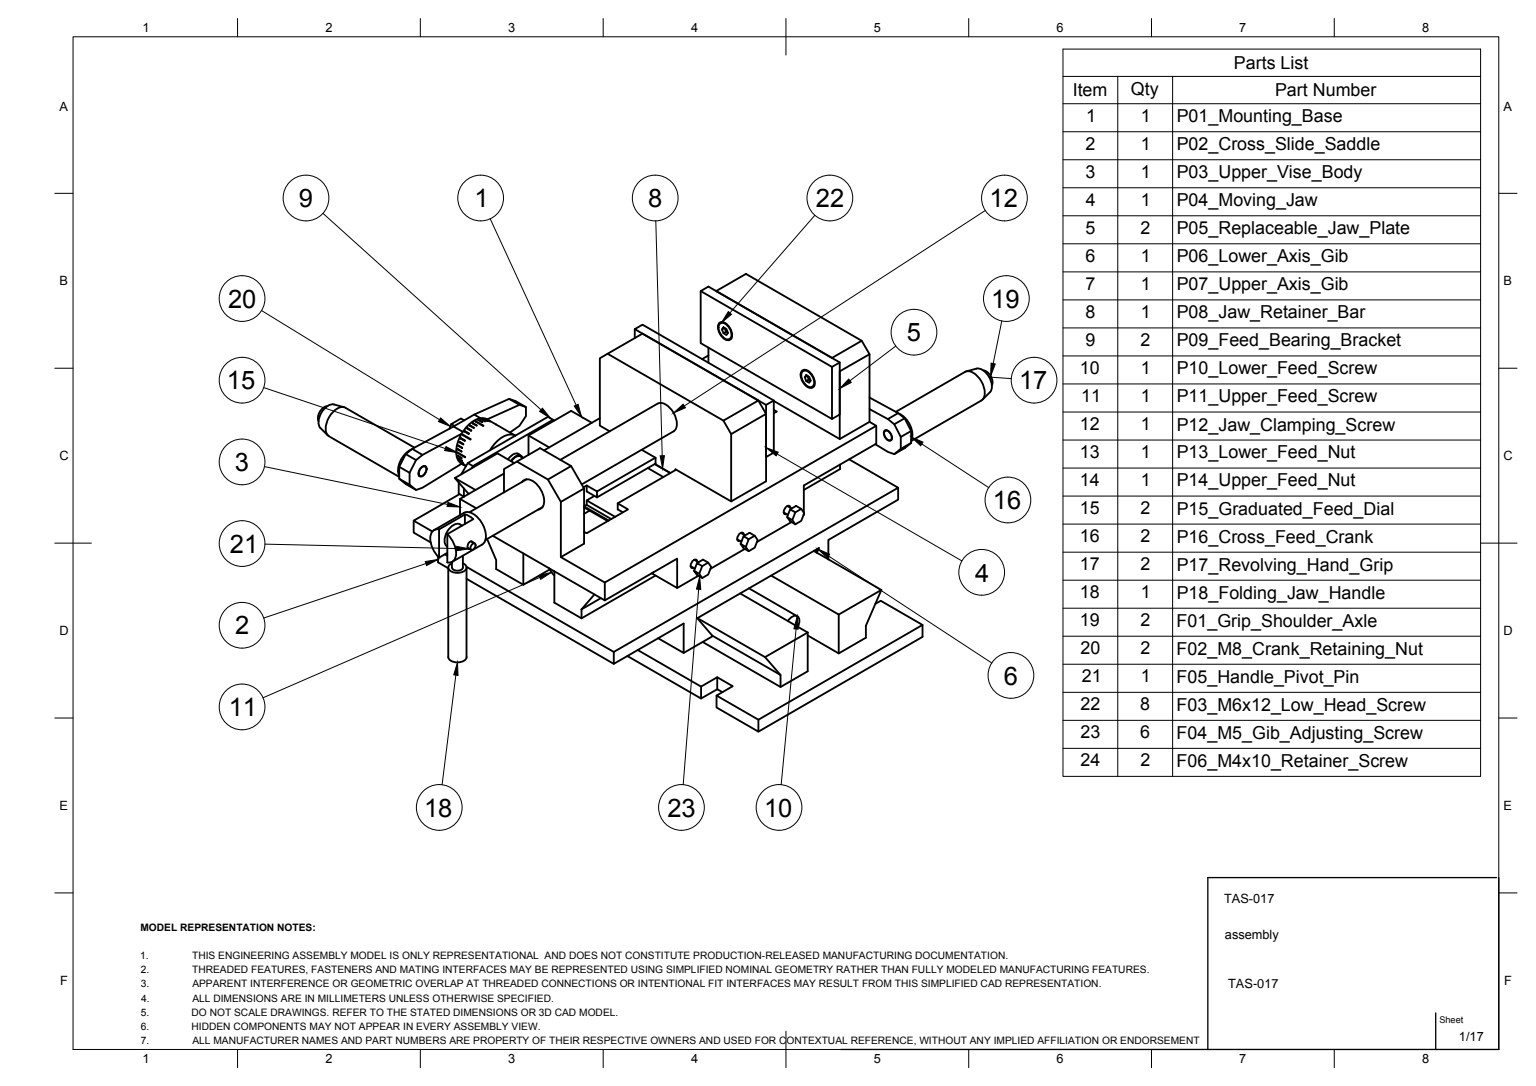
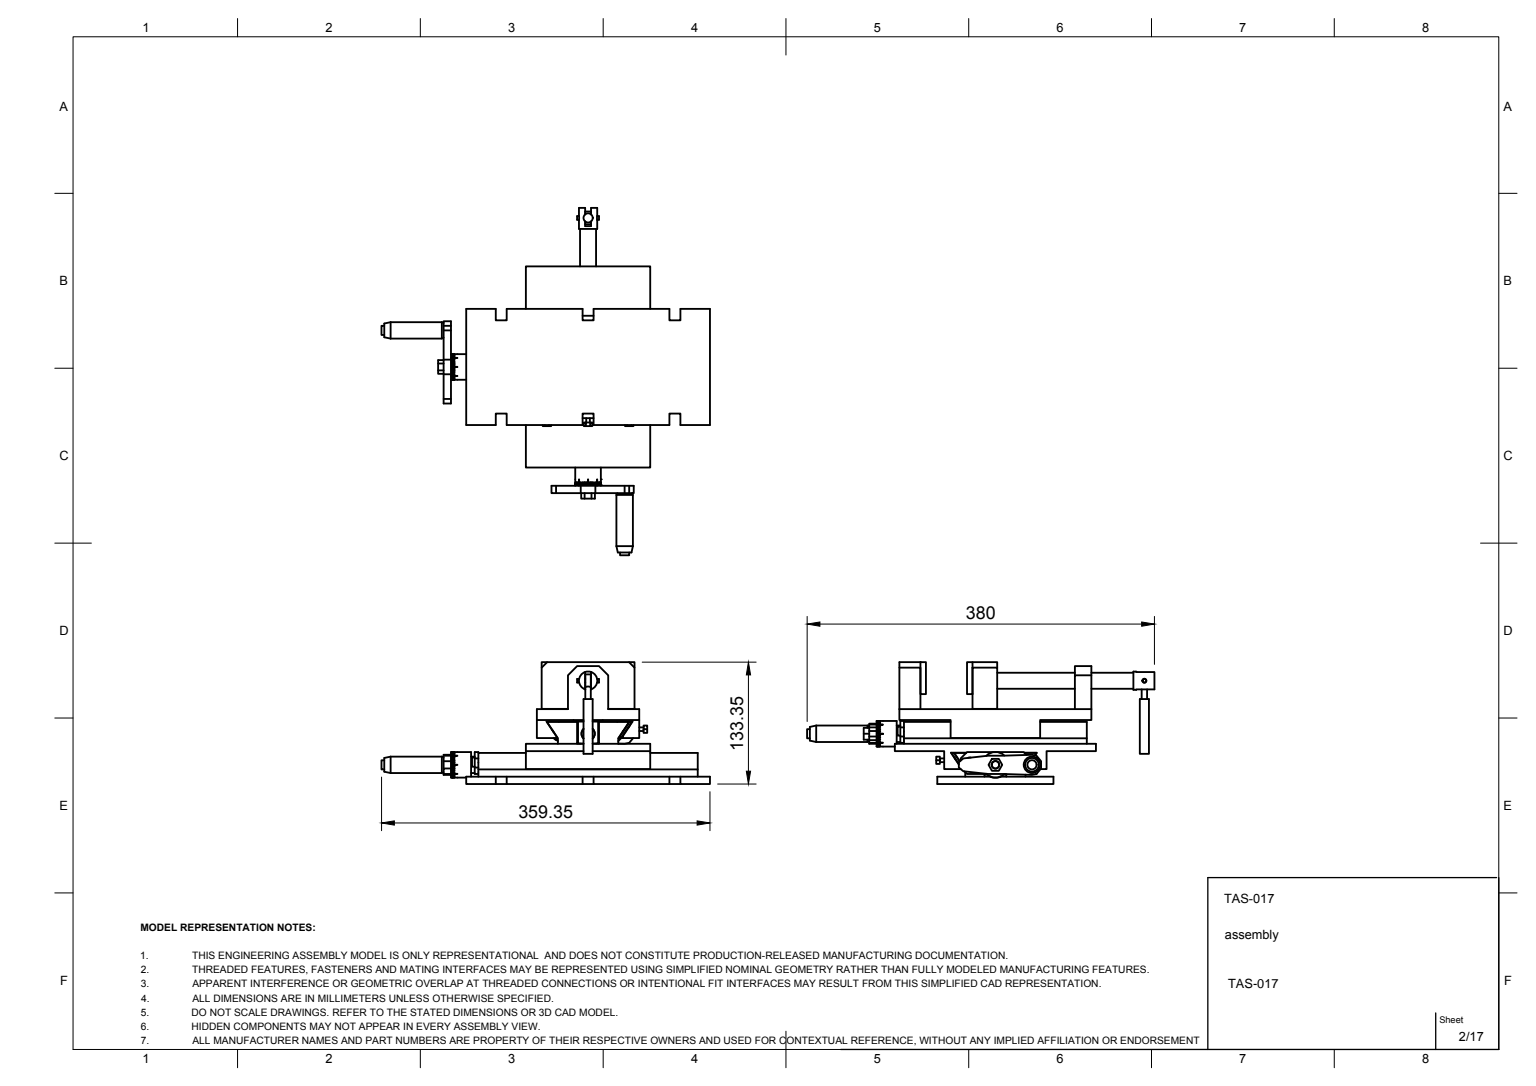
ISO-10303-21;
HEADER;
/* Generated by software containing ST-Developer
 * from STEP Tools, Inc. (www.steptools.com) 
 */

FILE_DESCRIPTION(
/* description */ ('STEP AP203'),
/* implementation_level */ '2;1');

FILE_NAME(
/* name */ 'TAS-017.step',
/* time_stamp */ '2026-11-15T15:04:01-08:00',
/* author */ (''),
/* organization */ (''),
/* preprocessor_version */ 'ST-DEVELOPER v20.2',
/* originating_system */ 'Autodesk Translation Framework v15.17.0.0',
/* authorisation */ '');

FILE_SCHEMA (('AUTOMOTIVE_DESIGN { 1 0 10303 214 3 1 1 }'));
ENDSEC;

DATA;
#10=MECHANICAL_DESIGN_GEOMETRIC_PRESENTATION_REPRESENTATION('',(#276,#277,
#278,#279,#280,#281,#282,#283,#284,#285,#286,#287,#288,#289,#290,#291,#292,
#293,#294,#295,#296,#297,#298,#299,#300,#301,#302,#303,#304,#305),#16598);
#11=ITEM_DEFINED_TRANSFORMATION($,$,#10077,#10884);
#12=ITEM_DEFINED_TRANSFORMATION($,$,#10132,#10885);
#13=ITEM_DEFINED_TRANSFORMATION($,$,#10189,#10886);
#14=ITEM_DEFINED_TRANSFORMATION($,$,#10266,#10887);
#15=ITEM_DEFINED_TRANSFORMATION($,$,#10446,#10888);
#16=ITEM_DEFINED_TRANSFORMATION($,$,#10299,#10889);
#17=ITEM_DEFINED_TRANSFORMATION($,$,#10306,#10890);
#18=ITEM_DEFINED_TRANSFORMATION($,$,#10313,#10891);
#19=ITEM_DEFINED_TRANSFORMATION($,$,#10467,#10892);
#20=ITEM_DEFINED_TRANSFORMATION($,$,#10334,#10893);
#21=ITEM_DEFINED_TRANSFORMATION($,$,#10356,#10894);
#22=ITEM_DEFINED_TRANSFORMATION($,$,#10378,#10895);
#23=ITEM_DEFINED_TRANSFORMATION($,$,#10404,#10896);
#24=ITEM_DEFINED_TRANSFORMATION($,$,#10414,#10897);
#25=ITEM_DEFINED_TRANSFORMATION($,$,#10487,#10898);
#26=ITEM_DEFINED_TRANSFORMATION($,$,#10778,#10899);
#27=ITEM_DEFINED_TRANSFORMATION($,$,#10801,#10900);
#28=ITEM_DEFINED_TRANSFORMATION($,$,#10424,#10901);
#29=ITEM_DEFINED_TRANSFORMATION($,$,#10815,#10902);
#30=ITEM_DEFINED_TRANSFORMATION($,$,#10825,#10903);
#31=ITEM_DEFINED_TRANSFORMATION($,$,#10440,#10904);
#32=ITEM_DEFINED_TRANSFORMATION($,$,#10837,#10905);
#33=ITEM_DEFINED_TRANSFORMATION($,$,#10854,#10906);
#34=ITEM_DEFINED_TRANSFORMATION($,$,#10867,#10907);
#35=ITEM_DEFINED_TRANSFORMATION($,$,#10446,#10908);
#36=ITEM_DEFINED_TRANSFORMATION($,$,#10467,#10909);
#37=ITEM_DEFINED_TRANSFORMATION($,$,#10487,#10910);
#38=ITEM_DEFINED_TRANSFORMATION($,$,#10778,#10911);
#39=ITEM_DEFINED_TRANSFORMATION($,$,#10801,#10912);
#40=ITEM_DEFINED_TRANSFORMATION($,$,#10815,#10913);
#41=ITEM_DEFINED_TRANSFORMATION($,$,#10825,#10914);
#42=ITEM_DEFINED_TRANSFORMATION($,$,#10837,#10915);
#43=ITEM_DEFINED_TRANSFORMATION($,$,#10837,#10916);
#44=ITEM_DEFINED_TRANSFORMATION($,$,#10837,#10917);
#45=ITEM_DEFINED_TRANSFORMATION($,$,#10837,#10918);
#46=ITEM_DEFINED_TRANSFORMATION($,$,#10837,#10919);
#47=ITEM_DEFINED_TRANSFORMATION($,$,#10837,#10920);
#48=ITEM_DEFINED_TRANSFORMATION($,$,#10837,#10921);
#49=ITEM_DEFINED_TRANSFORMATION($,$,#10854,#10922);
#50=ITEM_DEFINED_TRANSFORMATION($,$,#10854,#10923);
#51=ITEM_DEFINED_TRANSFORMATION($,$,#10854,#10924);
#52=ITEM_DEFINED_TRANSFORMATION($,$,#10854,#10925);
#53=ITEM_DEFINED_TRANSFORMATION($,$,#10854,#10926);
#54=ITEM_DEFINED_TRANSFORMATION($,$,#10867,#10927);
#55=(
REPRESENTATION_RELATIONSHIP($,$,#16698,#16697)
REPRESENTATION_RELATIONSHIP_WITH_TRANSFORMATION(#11)
SHAPE_REPRESENTATION_RELATIONSHIP()
);
#56=(
REPRESENTATION_RELATIONSHIP($,$,#16699,#16697)
REPRESENTATION_RELATIONSHIP_WITH_TRANSFORMATION(#12)
SHAPE_REPRESENTATION_RELATIONSHIP()
);
#57=(
REPRESENTATION_RELATIONSHIP($,$,#16700,#16697)
REPRESENTATION_RELATIONSHIP_WITH_TRANSFORMATION(#13)
SHAPE_REPRESENTATION_RELATIONSHIP()
);
#58=(
REPRESENTATION_RELATIONSHIP($,$,#16701,#16697)
REPRESENTATION_RELATIONSHIP_WITH_TRANSFORMATION(#14)
SHAPE_REPRESENTATION_RELATIONSHIP()
);
#59=(
REPRESENTATION_RELATIONSHIP($,$,#16712,#16697)
REPRESENTATION_RELATIONSHIP_WITH_TRANSFORMATION(#15)
SHAPE_REPRESENTATION_RELATIONSHIP()
);
#60=(
REPRESENTATION_RELATIONSHIP($,$,#16702,#16697)
REPRESENTATION_RELATIONSHIP_WITH_TRANSFORMATION(#16)
SHAPE_REPRESENTATION_RELATIONSHIP()
);
#61=(
REPRESENTATION_RELATIONSHIP($,$,#16703,#16697)
REPRESENTATION_RELATIONSHIP_WITH_TRANSFORMATION(#17)
SHAPE_REPRESENTATION_RELATIONSHIP()
);
#62=(
REPRESENTATION_RELATIONSHIP($,$,#16704,#16697)
REPRESENTATION_RELATIONSHIP_WITH_TRANSFORMATION(#18)
SHAPE_REPRESENTATION_RELATIONSHIP()
);
#63=(
REPRESENTATION_RELATIONSHIP($,$,#16713,#16697)
REPRESENTATION_RELATIONSHIP_WITH_TRANSFORMATION(#19)
SHAPE_REPRESENTATION_RELATIONSHIP()
);
#64=(
REPRESENTATION_RELATIONSHIP($,$,#16705,#16697)
REPRESENTATION_RELATIONSHIP_WITH_TRANSFORMATION(#20)
SHAPE_REPRESENTATION_RELATIONSHIP()
);
#65=(
REPRESENTATION_RELATIONSHIP($,$,#16706,#16697)
REPRESENTATION_RELATIONSHIP_WITH_TRANSFORMATION(#21)
SHAPE_REPRESENTATION_RELATIONSHIP()
);
#66=(
REPRESENTATION_RELATIONSHIP($,$,#16707,#16697)
REPRESENTATION_RELATIONSHIP_WITH_TRANSFORMATION(#22)
SHAPE_REPRESENTATION_RELATIONSHIP()
);
#67=(
REPRESENTATION_RELATIONSHIP($,$,#16708,#16697)
REPRESENTATION_RELATIONSHIP_WITH_TRANSFORMATION(#23)
SHAPE_REPRESENTATION_RELATIONSHIP()
);
#68=(
REPRESENTATION_RELATIONSHIP($,$,#16709,#16697)
REPRESENTATION_RELATIONSHIP_WITH_TRANSFORMATION(#24)
SHAPE_REPRESENTATION_RELATIONSHIP()
);
#69=(
REPRESENTATION_RELATIONSHIP($,$,#16714,#16697)
REPRESENTATION_RELATIONSHIP_WITH_TRANSFORMATION(#25)
SHAPE_REPRESENTATION_RELATIONSHIP()
);
#70=(
REPRESENTATION_RELATIONSHIP($,$,#16715,#16697)
REPRESENTATION_RELATIONSHIP_WITH_TRANSFORMATION(#26)
SHAPE_REPRESENTATION_RELATIONSHIP()
);
#71=(
REPRESENTATION_RELATIONSHIP($,$,#16716,#16697)
REPRESENTATION_RELATIONSHIP_WITH_TRANSFORMATION(#27)
SHAPE_REPRESENTATION_RELATIONSHIP()
);
#72=(
REPRESENTATION_RELATIONSHIP($,$,#16710,#16697)
REPRESENTATION_RELATIONSHIP_WITH_TRANSFORMATION(#28)
SHAPE_REPRESENTATION_RELATIONSHIP()
);
#73=(
REPRESENTATION_RELATIONSHIP($,$,#16717,#16697)
REPRESENTATION_RELATIONSHIP_WITH_TRANSFORMATION(#29)
SHAPE_REPRESENTATION_RELATIONSHIP()
);
#74=(
REPRESENTATION_RELATIONSHIP($,$,#16718,#16697)
REPRESENTATION_RELATIONSHIP_WITH_TRANSFORMATION(#30)
SHAPE_REPRESENTATION_RELATIONSHIP()
);
#75=(
REPRESENTATION_RELATIONSHIP($,$,#16711,#16697)
REPRESENTATION_RELATIONSHIP_WITH_TRANSFORMATION(#31)
SHAPE_REPRESENTATION_RELATIONSHIP()
);
#76=(
REPRESENTATION_RELATIONSHIP($,$,#16719,#16697)
REPRESENTATION_RELATIONSHIP_WITH_TRANSFORMATION(#32)
SHAPE_REPRESENTATION_RELATIONSHIP()
);
#77=(
REPRESENTATION_RELATIONSHIP($,$,#16720,#16697)
REPRESENTATION_RELATIONSHIP_WITH_TRANSFORMATION(#33)
SHAPE_REPRESENTATION_RELATIONSHIP()
);
#78=(
REPRESENTATION_RELATIONSHIP($,$,#16721,#16697)
REPRESENTATION_RELATIONSHIP_WITH_TRANSFORMATION(#34)
SHAPE_REPRESENTATION_RELATIONSHIP()
);
#79=(
REPRESENTATION_RELATIONSHIP($,$,#16712,#16697)
REPRESENTATION_RELATIONSHIP_WITH_TRANSFORMATION(#35)
SHAPE_REPRESENTATION_RELATIONSHIP()
);
#80=(
REPRESENTATION_RELATIONSHIP($,$,#16713,#16697)
REPRESENTATION_RELATIONSHIP_WITH_TRANSFORMATION(#36)
SHAPE_REPRESENTATION_RELATIONSHIP()
);
#81=(
REPRESENTATION_RELATIONSHIP($,$,#16714,#16697)
REPRESENTATION_RELATIONSHIP_WITH_TRANSFORMATION(#37)
SHAPE_REPRESENTATION_RELATIONSHIP()
);
#82=(
REPRESENTATION_RELATIONSHIP($,$,#16715,#16697)
REPRESENTATION_RELATIONSHIP_WITH_TRANSFORMATION(#38)
SHAPE_REPRESENTATION_RELATIONSHIP()
);
#83=(
REPRESENTATION_RELATIONSHIP($,$,#16716,#16697)
REPRESENTATION_RELATIONSHIP_WITH_TRANSFORMATION(#39)
SHAPE_REPRESENTATION_RELATIONSHIP()
);
#84=(
REPRESENTATION_RELATIONSHIP($,$,#16717,#16697)
REPRESENTATION_RELATIONSHIP_WITH_TRANSFORMATION(#40)
SHAPE_REPRESENTATION_RELATIONSHIP()
);
#85=(
REPRESENTATION_RELATIONSHIP($,$,#16718,#16697)
REPRESENTATION_RELATIONSHIP_WITH_TRANSFORMATION(#41)
SHAPE_REPRESENTATION_RELATIONSHIP()
);
#86=(
REPRESENTATION_RELATIONSHIP($,$,#16719,#16697)
REPRESENTATION_RELATIONSHIP_WITH_TRANSFORMATION(#42)
SHAPE_REPRESENTATION_RELATIONSHIP()
);
#87=(
REPRESENTATION_RELATIONSHIP($,$,#16719,#16697)
REPRESENTATION_RELATIONSHIP_WITH_TRANSFORMATION(#43)
SHAPE_REPRESENTATION_RELATIONSHIP()
);
#88=(
REPRESENTATION_RELATIONSHIP($,$,#16719,#16697)
REPRESENTATION_RELATIONSHIP_WITH_TRANSFORMATION(#44)
SHAPE_REPRESENTATION_RELATIONSHIP()
);
#89=(
REPRESENTATION_RELATIONSHIP($,$,#16719,#16697)
REPRESENTATION_RELATIONSHIP_WITH_TRANSFORMATION(#45)
SHAPE_REPRESENTATION_RELATIONSHIP()
);
#90=(
REPRESENTATION_RELATIONSHIP($,$,#16719,#16697)
REPRESENTATION_RELATIONSHIP_WITH_TRANSFORMATION(#46)
SHAPE_REPRESENTATION_RELATIONSHIP()
);
#91=(
REPRESENTATION_RELATIONSHIP($,$,#16719,#16697)
REPRESENTATION_RELATIONSHIP_WITH_TRANSFORMATION(#47)
SHAPE_REPRESENTATION_RELATIONSHIP()
);
#92=(
REPRESENTATION_RELATIONSHIP($,$,#16719,#16697)
REPRESENTATION_RELATIONSHIP_WITH_TRANSFORMATION(#48)
SHAPE_REPRESENTATION_RELATIONSHIP()
);
#93=(
REPRESENTATION_RELATIONSHIP($,$,#16720,#16697)
REPRESENTATION_RELATIONSHIP_WITH_TRANSFORMATION(#49)
SHAPE_REPRESENTATION_RELATIONSHIP()
);
#94=(
REPRESENTATION_RELATIONSHIP($,$,#16720,#16697)
REPRESENTATION_RELATIONSHIP_WITH_TRANSFORMATION(#50)
SHAPE_REPRESENTATION_RELATIONSHIP()
);
#95=(
REPRESENTATION_RELATIONSHIP($,$,#16720,#16697)
REPRESENTATION_RELATIONSHIP_WITH_TRANSFORMATION(#51)
SHAPE_REPRESENTATION_RELATIONSHIP()
);
#96=(
REPRESENTATION_RELATIONSHIP($,$,#16720,#16697)
REPRESENTATION_RELATIONSHIP_WITH_TRANSFORMATION(#52)
SHAPE_REPRESENTATION_RELATIONSHIP()
);
#97=(
REPRESENTATION_RELATIONSHIP($,$,#16720,#16697)
REPRESENTATION_RELATIONSHIP_WITH_TRANSFORMATION(#53)
SHAPE_REPRESENTATION_RELATIONSHIP()
);
#98=(
REPRESENTATION_RELATIONSHIP($,$,#16721,#16697)
REPRESENTATION_RELATIONSHIP_WITH_TRANSFORMATION(#54)
SHAPE_REPRESENTATION_RELATIONSHIP()
);
#99=CONTEXT_DEPENDENT_SHAPE_REPRESENTATION(#55,#16653);
#100=CONTEXT_DEPENDENT_SHAPE_REPRESENTATION(#56,#16654);
#101=CONTEXT_DEPENDENT_SHAPE_REPRESENTATION(#57,#16655);
#102=CONTEXT_DEPENDENT_SHAPE_REPRESENTATION(#58,#16656);
#103=CONTEXT_DEPENDENT_SHAPE_REPRESENTATION(#59,#16657);
#104=CONTEXT_DEPENDENT_SHAPE_REPRESENTATION(#60,#16658);
#105=CONTEXT_DEPENDENT_SHAPE_REPRESENTATION(#61,#16659);
#106=CONTEXT_DEPENDENT_SHAPE_REPRESENTATION(#62,#16660);
#107=CONTEXT_DEPENDENT_SHAPE_REPRESENTATION(#63,#16661);
#108=CONTEXT_DEPENDENT_SHAPE_REPRESENTATION(#64,#16662);
#109=CONTEXT_DEPENDENT_SHAPE_REPRESENTATION(#65,#16663);
#110=CONTEXT_DEPENDENT_SHAPE_REPRESENTATION(#66,#16664);
#111=CONTEXT_DEPENDENT_SHAPE_REPRESENTATION(#67,#16665);
#112=CONTEXT_DEPENDENT_SHAPE_REPRESENTATION(#68,#16666);
#113=CONTEXT_DEPENDENT_SHAPE_REPRESENTATION(#69,#16667);
#114=CONTEXT_DEPENDENT_SHAPE_REPRESENTATION(#70,#16668);
#115=CONTEXT_DEPENDENT_SHAPE_REPRESENTATION(#71,#16669);
#116=CONTEXT_DEPENDENT_SHAPE_REPRESENTATION(#72,#16670);
#117=CONTEXT_DEPENDENT_SHAPE_REPRESENTATION(#73,#16671);
#118=CONTEXT_DEPENDENT_SHAPE_REPRESENTATION(#74,#16672);
#119=CONTEXT_DEPENDENT_SHAPE_REPRESENTATION(#75,#16673);
#120=CONTEXT_DEPENDENT_SHAPE_REPRESENTATION(#76,#16674);
#121=CONTEXT_DEPENDENT_SHAPE_REPRESENTATION(#77,#16675);
#122=CONTEXT_DEPENDENT_SHAPE_REPRESENTATION(#78,#16676);
#123=CONTEXT_DEPENDENT_SHAPE_REPRESENTATION(#79,#16677);
#124=CONTEXT_DEPENDENT_SHAPE_REPRESENTATION(#80,#16678);
#125=CONTEXT_DEPENDENT_SHAPE_REPRESENTATION(#81,#16679);
#126=CONTEXT_DEPENDENT_SHAPE_REPRESENTATION(#82,#16680);
#127=CONTEXT_DEPENDENT_SHAPE_REPRESENTATION(#83,#16681);
#128=CONTEXT_DEPENDENT_SHAPE_REPRESENTATION(#84,#16682);
#129=CONTEXT_DEPENDENT_SHAPE_REPRESENTATION(#85,#16683);
#130=CONTEXT_DEPENDENT_SHAPE_REPRESENTATION(#86,#16684);
#131=CONTEXT_DEPENDENT_SHAPE_REPRESENTATION(#87,#16685);
#132=CONTEXT_DEPENDENT_SHAPE_REPRESENTATION(#88,#16686);
#133=CONTEXT_DEPENDENT_SHAPE_REPRESENTATION(#89,#16687);
#134=CONTEXT_DEPENDENT_SHAPE_REPRESENTATION(#90,#16688);
#135=CONTEXT_DEPENDENT_SHAPE_REPRESENTATION(#91,#16689);
#136=CONTEXT_DEPENDENT_SHAPE_REPRESENTATION(#92,#16690);
#137=CONTEXT_DEPENDENT_SHAPE_REPRESENTATION(#93,#16691);
#138=CONTEXT_DEPENDENT_SHAPE_REPRESENTATION(#94,#16692);
#139=CONTEXT_DEPENDENT_SHAPE_REPRESENTATION(#95,#16693);
#140=CONTEXT_DEPENDENT_SHAPE_REPRESENTATION(#96,#16694);
#141=CONTEXT_DEPENDENT_SHAPE_REPRESENTATION(#97,#16695);
#142=CONTEXT_DEPENDENT_SHAPE_REPRESENTATION(#98,#16696);
#143=NEXT_ASSEMBLY_USAGE_OCCURRENCE('P01_Mounting_Base:1',
'P01_Mounting_Base:1','P01_Mounting_Base:1',#16723,#16724,
'P01_Mounting_Base:1');
#144=NEXT_ASSEMBLY_USAGE_OCCURRENCE('P02_Cross_Slide_Saddle:1',
'P02_Cross_Slide_Saddle:1','P02_Cross_Slide_Saddle:1',#16723,#16725,
'P02_Cross_Slide_Saddle:1');
#145=NEXT_ASSEMBLY_USAGE_OCCURRENCE('P03_Upper_Vise_Body:1',
'P03_Upper_Vise_Body:1','P03_Upper_Vise_Body:1',#16723,#16726,
'P03_Upper_Vise_Body:1');
#146=NEXT_ASSEMBLY_USAGE_OCCURRENCE('P04_Moving_Jaw:1',
'P04_Moving_Jaw:1','P04_Moving_Jaw:1',#16723,#16727,'P04_Moving_Jaw:1');
#147=NEXT_ASSEMBLY_USAGE_OCCURRENCE('P05_Replaceable_Jaw_Plate:1',
'P05_Replaceable_Jaw_Plate:1','P05_Replaceable_Jaw_Plate:1',#16723,#16738,
'P05_Replaceable_Jaw_Plate:1');
#148=NEXT_ASSEMBLY_USAGE_OCCURRENCE('P06_Lower_Axis_Gib:1',
'P06_Lower_Axis_Gib:1','P06_Lower_Axis_Gib:1',#16723,#16728,
'P06_Lower_Axis_Gib:1');
#149=NEXT_ASSEMBLY_USAGE_OCCURRENCE('P07_Upper_Axis_Gib:1',
'P07_Upper_Axis_Gib:1','P07_Upper_Axis_Gib:1',#16723,#16729,
'P07_Upper_Axis_Gib:1');
#150=NEXT_ASSEMBLY_USAGE_OCCURRENCE('P08_Jaw_Retainer_Bar:1',
'P08_Jaw_Retainer_Bar:1','P08_Jaw_Retainer_Bar:1',#16723,#16730,
'P08_Jaw_Retainer_Bar:1');
#151=NEXT_ASSEMBLY_USAGE_OCCURRENCE('P09_Feed_Bearing_Bracket:1',
'P09_Feed_Bearing_Bracket:1','P09_Feed_Bearing_Bracket:1',#16723,#16739,
'P09_Feed_Bearing_Bracket:1');
#152=NEXT_ASSEMBLY_USAGE_OCCURRENCE('P10_Lower_Feed_Screw:1',
'P10_Lower_Feed_Screw:1','P10_Lower_Feed_Screw:1',#16723,#16731,
'P10_Lower_Feed_Screw:1');
#153=NEXT_ASSEMBLY_USAGE_OCCURRENCE('P11_Upper_Feed_Screw:1',
'P11_Upper_Feed_Screw:1','P11_Upper_Feed_Screw:1',#16723,#16732,
'P11_Upper_Feed_Screw:1');
#154=NEXT_ASSEMBLY_USAGE_OCCURRENCE('P12_Jaw_Clamping_Screw:1',
'P12_Jaw_Clamping_Screw:1','P12_Jaw_Clamping_Screw:1',#16723,#16733,
'P12_Jaw_Clamping_Screw:1');
#155=NEXT_ASSEMBLY_USAGE_OCCURRENCE('P13_Lower_Feed_Nut:1',
'P13_Lower_Feed_Nut:1','P13_Lower_Feed_Nut:1',#16723,#16734,
'P13_Lower_Feed_Nut:1');
#156=NEXT_ASSEMBLY_USAGE_OCCURRENCE('P14_Upper_Feed_Nut:1',
'P14_Upper_Feed_Nut:1','P14_Upper_Feed_Nut:1',#16723,#16735,
'P14_Upper_Feed_Nut:1');
#157=NEXT_ASSEMBLY_USAGE_OCCURRENCE('P15_Graduated_Feed_Dial:1',
'P15_Graduated_Feed_Dial:1','P15_Graduated_Feed_Dial:1',#16723,#16740,
'P15_Graduated_Feed_Dial:1');
#158=NEXT_ASSEMBLY_USAGE_OCCURRENCE('P16_Cross_Feed_Crank:1',
'P16_Cross_Feed_Crank:1','P16_Cross_Feed_Crank:1',#16723,#16741,
'P16_Cross_Feed_Crank:1');
#159=NEXT_ASSEMBLY_USAGE_OCCURRENCE('P17_Revolving_Hand_Grip:1',
'P17_Revolving_Hand_Grip:1','P17_Revolving_Hand_Grip:1',#16723,#16742,
'P17_Revolving_Hand_Grip:1');
#160=NEXT_ASSEMBLY_USAGE_OCCURRENCE('P18_Folding_Jaw_Handle:1',
'P18_Folding_Jaw_Handle:1','P18_Folding_Jaw_Handle:1',#16723,#16736,
'P18_Folding_Jaw_Handle:1');
#161=NEXT_ASSEMBLY_USAGE_OCCURRENCE('F01_Grip_Shoulder_Axle:1',
'F01_Grip_Shoulder_Axle:1','F01_Grip_Shoulder_Axle:1',#16723,#16743,
'F01_Grip_Shoulder_Axle:1');
#162=NEXT_ASSEMBLY_USAGE_OCCURRENCE('F02_M8_Crank_Retaining_Nut:1',
'F02_M8_Crank_Retaining_Nut:1','F02_M8_Crank_Retaining_Nut:1',#16723,#16744,
'F02_M8_Crank_Retaining_Nut:1');
#163=NEXT_ASSEMBLY_USAGE_OCCURRENCE('F05_Handle_Pivot_Pin:1',
'F05_Handle_Pivot_Pin:1','F05_Handle_Pivot_Pin:1',#16723,#16737,
'F05_Handle_Pivot_Pin:1');
#164=NEXT_ASSEMBLY_USAGE_OCCURRENCE('F03_M6x12_Low_Head_Screw:1',
'F03_M6x12_Low_Head_Screw:1','F03_M6x12_Low_Head_Screw:1',#16723,#16745,
'F03_M6x12_Low_Head_Screw:1');
#165=NEXT_ASSEMBLY_USAGE_OCCURRENCE('F04_M5_Gib_Adjusting_Screw:1',
'F04_M5_Gib_Adjusting_Screw:1','F04_M5_Gib_Adjusting_Screw:1',#16723,#16746,
'F04_M5_Gib_Adjusting_Screw:1');
#166=NEXT_ASSEMBLY_USAGE_OCCURRENCE('F06_M4x10_Retainer_Screw:1',
'F06_M4x10_Retainer_Screw:1','F06_M4x10_Retainer_Screw:1',#16723,#16747,
'F06_M4x10_Retainer_Screw:1');
#167=NEXT_ASSEMBLY_USAGE_OCCURRENCE('P05_Replaceable_Jaw_Plate:2',
'P05_Replaceable_Jaw_Plate:2','P05_Replaceable_Jaw_Plate:2',#16723,#16738,
'P05_Replaceable_Jaw_Plate:2');
#168=NEXT_ASSEMBLY_USAGE_OCCURRENCE('P09_Feed_Bearing_Bracket:2',
'P09_Feed_Bearing_Bracket:2','P09_Feed_Bearing_Bracket:2',#16723,#16739,
'P09_Feed_Bearing_Bracket:2');
#169=NEXT_ASSEMBLY_USAGE_OCCURRENCE('P15_Graduated_Feed_Dial:2',
'P15_Graduated_Feed_Dial:2','P15_Graduated_Feed_Dial:2',#16723,#16740,
'P15_Graduated_Feed_Dial:2');
#170=NEXT_ASSEMBLY_USAGE_OCCURRENCE('P16_Cross_Feed_Crank:2',
'P16_Cross_Feed_Crank:2','P16_Cross_Feed_Crank:2',#16723,#16741,
'P16_Cross_Feed_Crank:2');
#171=NEXT_ASSEMBLY_USAGE_OCCURRENCE('P17_Revolving_Hand_Grip:2',
'P17_Revolving_Hand_Grip:2','P17_Revolving_Hand_Grip:2',#16723,#16742,
'P17_Revolving_Hand_Grip:2');
#172=NEXT_ASSEMBLY_USAGE_OCCURRENCE('F01_Grip_Shoulder_Axle:2',
'F01_Grip_Shoulder_Axle:2','F01_Grip_Shoulder_Axle:2',#16723,#16743,
'F01_Grip_Shoulder_Axle:2');
#173=NEXT_ASSEMBLY_USAGE_OCCURRENCE('F02_M8_Crank_Retaining_Nut:2',
'F02_M8_Crank_Retaining_Nut:2','F02_M8_Crank_Retaining_Nut:2',#16723,#16744,
'F02_M8_Crank_Retaining_Nut:2');
#174=NEXT_ASSEMBLY_USAGE_OCCURRENCE('F03_M6x12_Low_Head_Screw:2',
'F03_M6x12_Low_Head_Screw:2','F03_M6x12_Low_Head_Screw:2',#16723,#16745,
'F03_M6x12_Low_Head_Screw:2');
#175=NEXT_ASSEMBLY_USAGE_OCCURRENCE('F03_M6x12_Low_Head_Screw:3',
'F03_M6x12_Low_Head_Screw:3','F03_M6x12_Low_Head_Screw:3',#16723,#16745,
'F03_M6x12_Low_Head_Screw:3');
#176=NEXT_ASSEMBLY_USAGE_OCCURRENCE('F03_M6x12_Low_Head_Screw:4',
'F03_M6x12_Low_Head_Screw:4','F03_M6x12_Low_Head_Screw:4',#16723,#16745,
'F03_M6x12_Low_Head_Screw:4');
#177=NEXT_ASSEMBLY_USAGE_OCCURRENCE('F03_M6x12_Low_Head_Screw:5',
'F03_M6x12_Low_Head_Screw:5','F03_M6x12_Low_Head_Screw:5',#16723,#16745,
'F03_M6x12_Low_Head_Screw:5');
#178=NEXT_ASSEMBLY_USAGE_OCCURRENCE('F03_M6x12_Low_Head_Screw:6',
'F03_M6x12_Low_Head_Screw:6','F03_M6x12_Low_Head_Screw:6',#16723,#16745,
'F03_M6x12_Low_Head_Screw:6');
#179=NEXT_ASSEMBLY_USAGE_OCCURRENCE('F03_M6x12_Low_Head_Screw:7',
'F03_M6x12_Low_Head_Screw:7','F03_M6x12_Low_Head_Screw:7',#16723,#16745,
'F03_M6x12_Low_Head_Screw:7');
#180=NEXT_ASSEMBLY_USAGE_OCCURRENCE('F03_M6x12_Low_Head_Screw:8',
'F03_M6x12_Low_Head_Screw:8','F03_M6x12_Low_Head_Screw:8',#16723,#16745,
'F03_M6x12_Low_Head_Screw:8');
#181=NEXT_ASSEMBLY_USAGE_OCCURRENCE('F04_M5_Gib_Adjusting_Screw:2',
'F04_M5_Gib_Adjusting_Screw:2','F04_M5_Gib_Adjusting_Screw:2',#16723,#16746,
'F04_M5_Gib_Adjusting_Screw:2');
#182=NEXT_ASSEMBLY_USAGE_OCCURRENCE('F04_M5_Gib_Adjusting_Screw:3',
'F04_M5_Gib_Adjusting_Screw:3','F04_M5_Gib_Adjusting_Screw:3',#16723,#16746,
'F04_M5_Gib_Adjusting_Screw:3');
#183=NEXT_ASSEMBLY_USAGE_OCCURRENCE('F04_M5_Gib_Adjusting_Screw:4',
'F04_M5_Gib_Adjusting_Screw:4','F04_M5_Gib_Adjusting_Screw:4',#16723,#16746,
'F04_M5_Gib_Adjusting_Screw:4');
#184=NEXT_ASSEMBLY_USAGE_OCCURRENCE('F04_M5_Gib_Adjusting_Screw:5',
'F04_M5_Gib_Adjusting_Screw:5','F04_M5_Gib_Adjusting_Screw:5',#16723,#16746,
'F04_M5_Gib_Adjusting_Screw:5');
#185=NEXT_ASSEMBLY_USAGE_OCCURRENCE('F04_M5_Gib_Adjusting_Screw:6',
'F04_M5_Gib_Adjusting_Screw:6','F04_M5_Gib_Adjusting_Screw:6',#16723,#16746,
'F04_M5_Gib_Adjusting_Screw:6');
#186=NEXT_ASSEMBLY_USAGE_OCCURRENCE('F06_M4x10_Retainer_Screw:2',
'F06_M4x10_Retainer_Screw:2','F06_M4x10_Retainer_Screw:2',#16723,#16747,
'F06_M4x10_Retainer_Screw:2');
#187=CONICAL_SURFACE('',#10802,7.5,0.211093333222747);
#188=CONICAL_SURFACE('',#10808,9.,0.463647609000806);
#189=B_SPLINE_CURVE_WITH_KNOTS('',3,(#14759,#14760,#14761,#14762,#14763,
#14764,#14765,#14766,#14767,#14768,#14769,#14770,#14771,#14772,#14773,#14774,
#14775,#14776),.UNSPECIFIED.,.F.,.F.,(4,2,2,2,2,2,2,2,4),(1.66329163352374,
1.74645277590797,1.82961391829221,1.91278193926035,1.99594996022848,2.07911798119662,
2.16228600216475,2.24544714454899,2.32860828693323),.UNSPECIFIED.);
#190=B_SPLINE_CURVE_WITH_KNOTS('',3,(#14777,#14778,#14779,#14780,#14781,
#14782,#14783,#14784,#14785,#14786,#14787,#14788,#14789,#14790,#14791,#14792,
#14793,#14794,#14795),.UNSPECIFIED.,.F.,.F.,(4,2,2,2,3,2,2,2,4),(0.997974980114241,
1.08113612249848,1.16429726488272,1.24746528585085,1.33063330681899,1.41380132778712,
1.49696934875526,1.5801304911395,1.66329163352374),.UNSPECIFIED.);
#191=B_SPLINE_CURVE_WITH_KNOTS('',3,(#14799,#14800,#14801,#14802,#14803,
#14804,#14805,#14806,#14807,#14808,#14809,#14810,#14811,#14812,#14813,#14814,
#14815,#14816),.UNSPECIFIED.,.F.,.F.,(4,2,2,2,2,2,2,2,4),(-0.997974980114241,
-0.914813837730002,-0.831652695345763,-0.748484674377629,-0.665316653409494,
-0.58214863244136,-0.498980611473225,-0.415819469088986,-0.332658326704747),
 .UNSPECIFIED.);
#192=B_SPLINE_CURVE_WITH_KNOTS('',3,(#14820,#14821,#14822,#14823,#14824,
#14825,#14826,#14827,#14828,#14829,#14830,#14831,#14832,#14833,#14834,#14835,
#14836,#14837,#14838),.UNSPECIFIED.,.F.,.F.,(4,2,2,2,3,2,2,2,4),(-0.332658326704747,
-0.249497184320508,-0.166336041936269,-0.0831680209681343,0.,0.0831680209681345,
0.166336041936269,0.249497184320508,0.332658326704747),.UNSPECIFIED.);
#193=B_SPLINE_CURVE_WITH_KNOTS('',3,(#14963,#14964,#14965,#14966,#14967,
#14968,#14969,#14970,#14971,#14972,#14973,#14974,#14975,#14976,#14977,#14978,
#14979,#14980),.UNSPECIFIED.,.F.,.F.,(4,2,2,2,2,2,2,2,4),(0.458554765704034,
0.573115036583473,0.687675307462911,0.80239241943549,0.917109531408068,
1.03182664338065,1.14654375535323,1.26110402623266,1.3756642971121),
 .UNSPECIFIED.);
#194=B_SPLINE_CURVE_WITH_KNOTS('',3,(#14982,#14983,#14984,#14985,#14986,
#14987,#14988,#14989,#14990,#14991,#14992,#14993,#14994,#14995,#14996,#14997,
#14998,#14999,#15000),.UNSPECIFIED.,.F.,.F.,(4,2,2,2,3,2,2,2,4),(-0.458554765704034,
-0.343994494824596,-0.229434223945157,-0.114717111972579,0.,0.114717111972579,
0.229434223945157,0.343994494824596,0.458554765704034),.UNSPECIFIED.);
#195=ELLIPSE('',#10144,3.12481110540129,2.59999999999927);
#196=ELLIPSE('',#10146,3.12481110540129,2.59999999999927);
#197=ELLIPSE('',#10149,3.12481110540191,2.59999999999976);
#198=ELLIPSE('',#10151,3.12481110540191,2.59999999999976);
#199=ELLIPSE('',#10154,3.1248111054022,2.60000000000004);
#200=ELLIPSE('',#10156,3.1248111054022,2.60000000000004);
#201=ELLIPSE('',#10193,3.12481110540202,2.59999999999971);
#202=ELLIPSE('',#10198,3.1248111054012,2.59999999999909);
#203=ELLIPSE('',#10203,3.12481110540162,2.59999999999945);
#204=SHAPE_REPRESENTATION_RELATIONSHIP('SRR','None',#16698,#228);
#205=SHAPE_REPRESENTATION_RELATIONSHIP('SRR','None',#16699,#229);
#206=SHAPE_REPRESENTATION_RELATIONSHIP('SRR','None',#16700,#230);
#207=SHAPE_REPRESENTATION_RELATIONSHIP('SRR','None',#16701,#231);
#208=SHAPE_REPRESENTATION_RELATIONSHIP('SRR','None',#16702,#232);
#209=SHAPE_REPRESENTATION_RELATIONSHIP('SRR','None',#16703,#233);
#210=SHAPE_REPRESENTATION_RELATIONSHIP('SRR','None',#16704,#234);
#211=SHAPE_REPRESENTATION_RELATIONSHIP('SRR','None',#16705,#235);
#212=SHAPE_REPRESENTATION_RELATIONSHIP('SRR','None',#16706,#236);
#213=SHAPE_REPRESENTATION_RELATIONSHIP('SRR','None',#16707,#237);
#214=SHAPE_REPRESENTATION_RELATIONSHIP('SRR','None',#16708,#238);
#215=SHAPE_REPRESENTATION_RELATIONSHIP('SRR','None',#16709,#239);
#216=SHAPE_REPRESENTATION_RELATIONSHIP('SRR','None',#16710,#240);
#217=SHAPE_REPRESENTATION_RELATIONSHIP('SRR','None',#16711,#241);
#218=SHAPE_REPRESENTATION_RELATIONSHIP('SRR','None',#16712,#242);
#219=SHAPE_REPRESENTATION_RELATIONSHIP('SRR','None',#16713,#243);
#220=SHAPE_REPRESENTATION_RELATIONSHIP('SRR','None',#16714,#244);
#221=SHAPE_REPRESENTATION_RELATIONSHIP('SRR','None',#16715,#245);
#222=SHAPE_REPRESENTATION_RELATIONSHIP('SRR','None',#16716,#246);
#223=SHAPE_REPRESENTATION_RELATIONSHIP('SRR','None',#16717,#247);
#224=SHAPE_REPRESENTATION_RELATIONSHIP('SRR','None',#16718,#248);
#225=SHAPE_REPRESENTATION_RELATIONSHIP('SRR','None',#16719,#249);
#226=SHAPE_REPRESENTATION_RELATIONSHIP('SRR','None',#16720,#250);
#227=SHAPE_REPRESENTATION_RELATIONSHIP('SRR','None',#16721,#251);
#228=ADVANCED_BREP_SHAPE_REPRESENTATION('',(#252),#16574);
#229=ADVANCED_BREP_SHAPE_REPRESENTATION('',(#253),#16575);
#230=ADVANCED_BREP_SHAPE_REPRESENTATION('',(#254),#16576);
#231=ADVANCED_BREP_SHAPE_REPRESENTATION('',(#255),#16577);
#232=ADVANCED_BREP_SHAPE_REPRESENTATION('',(#256),#16578);
#233=ADVANCED_BREP_SHAPE_REPRESENTATION('',(#257),#16579);
#234=ADVANCED_BREP_SHAPE_REPRESENTATION('',(#258),#16580);
#235=ADVANCED_BREP_SHAPE_REPRESENTATION('',(#259),#16581);
#236=ADVANCED_BREP_SHAPE_REPRESENTATION('',(#260),#16582);
#237=ADVANCED_BREP_SHAPE_REPRESENTATION('',(#261),#16583);
#238=ADVANCED_BREP_SHAPE_REPRESENTATION('',(#262),#16584);
#239=ADVANCED_BREP_SHAPE_REPRESENTATION('',(#263),#16585);
#240=ADVANCED_BREP_SHAPE_REPRESENTATION('',(#264),#16586);
#241=ADVANCED_BREP_SHAPE_REPRESENTATION('',(#265),#16587);
#242=ADVANCED_BREP_SHAPE_REPRESENTATION('',(#266),#16588);
#243=ADVANCED_BREP_SHAPE_REPRESENTATION('',(#267),#16589);
#244=ADVANCED_BREP_SHAPE_REPRESENTATION('',(#268),#16590);
#245=ADVANCED_BREP_SHAPE_REPRESENTATION('',(#269),#16591);
#246=ADVANCED_BREP_SHAPE_REPRESENTATION('',(#270),#16592);
#247=ADVANCED_BREP_SHAPE_REPRESENTATION('',(#271),#16593);
#248=ADVANCED_BREP_SHAPE_REPRESENTATION('',(#272),#16594);
#249=ADVANCED_BREP_SHAPE_REPRESENTATION('',(#273),#16595);
#250=ADVANCED_BREP_SHAPE_REPRESENTATION('',(#274),#16596);
#251=ADVANCED_BREP_SHAPE_REPRESENTATION('',(#275),#16597);
#252=MANIFOLD_SOLID_BREP('Body1',#9787);
#253=MANIFOLD_SOLID_BREP('Body1',#9788);
#254=MANIFOLD_SOLID_BREP('Body1',#9789);
#255=MANIFOLD_SOLID_BREP('Body1',#9790);
#256=MANIFOLD_SOLID_BREP('Body1',#9791);
#257=MANIFOLD_SOLID_BREP('Body1',#9792);
#258=MANIFOLD_SOLID_BREP('Body1',#9793);
#259=MANIFOLD_SOLID_BREP('Body1',#9794);
#260=MANIFOLD_SOLID_BREP('Body1',#9795);
#261=MANIFOLD_SOLID_BREP('Body1',#9796);
#262=MANIFOLD_SOLID_BREP('Body1',#9797);
#263=MANIFOLD_SOLID_BREP('Body1',#9798);
#264=MANIFOLD_SOLID_BREP('Body1',#9799);
#265=MANIFOLD_SOLID_BREP('Body1',#9800);
#266=MANIFOLD_SOLID_BREP('Body1',#9801);
#267=MANIFOLD_SOLID_BREP('Body1',#9802);
#268=MANIFOLD_SOLID_BREP('Body1',#9803);
#269=MANIFOLD_SOLID_BREP('Body1',#9804);
#270=MANIFOLD_SOLID_BREP('Body1',#9805);
#271=MANIFOLD_SOLID_BREP('Body1',#9806);
#272=MANIFOLD_SOLID_BREP('Body1',#9807);
#273=MANIFOLD_SOLID_BREP('Body1',#9808);
#274=MANIFOLD_SOLID_BREP('Body1',#9809);
#275=MANIFOLD_SOLID_BREP('Body1',#9810);
#276=STYLED_ITEM('',(#16828),#9252);
#277=STYLED_ITEM('',(#16828),#9258);
#278=STYLED_ITEM('',(#16827),#252);
#279=STYLED_ITEM('',(#16828),#9306);
#280=STYLED_ITEM('',(#16828),#9312);
#281=STYLED_ITEM('',(#16829),#253);
#282=STYLED_ITEM('',(#16830),#254);
#283=STYLED_ITEM('',(#16828),#9385);
#284=STYLED_ITEM('',(#16828),#9386);
#285=STYLED_ITEM('',(#16831),#255);
#286=STYLED_ITEM('',(#16827),#256);
#287=STYLED_ITEM('',(#16832),#257);
#288=STYLED_ITEM('',(#16833),#258);
#289=STYLED_ITEM('',(#16831),#259);
#290=STYLED_ITEM('',(#16832),#260);
#291=STYLED_ITEM('',(#16833),#261);
#292=STYLED_ITEM('',(#16834),#262);
#293=STYLED_ITEM('',(#16830),#263);
#294=STYLED_ITEM('',(#16832),#264);
#295=STYLED_ITEM('',(#16830),#265);
#296=STYLED_ITEM('',(#16834),#266);
#297=STYLED_ITEM('',(#16833),#267);
#298=STYLED_ITEM('',(#16834),#268);
#299=STYLED_ITEM('',(#16830),#269);
#300=STYLED_ITEM('',(#16827),#270);
#301=STYLED_ITEM('',(#16829),#271);
#302=STYLED_ITEM('',(#16833),#272);
#303=STYLED_ITEM('',(#16829),#273);
#304=STYLED_ITEM('',(#16832),#274);
#305=STYLED_ITEM('',(#16831),#275);
#306=FACE_BOUND('',#1465,.T.);
#307=FACE_BOUND('',#1466,.T.);
#308=FACE_BOUND('',#1484,.T.);
#309=FACE_BOUND('',#1491,.T.);
#310=FACE_BOUND('',#1521,.T.);
#311=FACE_BOUND('',#1522,.T.);
#312=FACE_BOUND('',#1524,.T.);
#313=FACE_BOUND('',#1525,.T.);
#314=FACE_BOUND('',#1526,.T.);
#315=FACE_BOUND('',#1535,.T.);
#316=FACE_BOUND('',#1536,.T.);
#317=FACE_BOUND('',#1537,.T.);
#318=FACE_BOUND('',#1547,.T.);
#319=FACE_BOUND('',#1554,.T.);
#320=FACE_BOUND('',#1569,.T.);
#321=FACE_BOUND('',#1583,.T.);
#322=FACE_BOUND('',#1584,.T.);
#323=FACE_BOUND('',#1585,.T.);
#324=FACE_BOUND('',#1587,.T.);
#325=FACE_BOUND('',#1588,.T.);
#326=FACE_BOUND('',#1589,.T.);
#327=FACE_BOUND('',#1597,.T.);
#328=FACE_BOUND('',#1606,.T.);
#329=FACE_BOUND('',#1607,.T.);
#330=FACE_BOUND('',#1614,.T.);
#331=FACE_BOUND('',#1644,.T.);
#332=FACE_BOUND('',#1645,.T.);
#333=FACE_BOUND('',#1647,.T.);
#334=FACE_BOUND('',#1651,.T.);
#335=FACE_BOUND('',#1652,.T.);
#336=FACE_BOUND('',#1679,.T.);
#337=FACE_BOUND('',#1680,.T.);
#338=FACE_BOUND('',#1682,.T.);
#339=FACE_BOUND('',#1683,.T.);
#340=FACE_BOUND('',#1685,.T.);
#341=FACE_BOUND('',#1687,.T.);
#342=FACE_BOUND('',#1695,.T.);
#343=FACE_BOUND('',#1697,.T.);
#344=FACE_BOUND('',#1699,.T.);
#345=FACE_BOUND('',#1701,.T.);
#346=FACE_BOUND('',#1710,.T.);
#347=FACE_BOUND('',#1712,.T.);
#348=FACE_BOUND('',#1714,.T.);
#349=FACE_BOUND('',#1716,.T.);
#350=FACE_BOUND('',#1723,.T.);
#351=FACE_BOUND('',#1727,.T.);
#352=FACE_BOUND('',#1729,.T.);
#353=FACE_BOUND('',#1732,.T.);
#354=FACE_BOUND('',#1734,.T.);
#355=FACE_BOUND('',#1738,.T.);
#356=FACE_BOUND('',#1740,.T.);
#357=FACE_BOUND('',#1747,.T.);
#358=FACE_BOUND('',#1749,.T.);
#359=FACE_BOUND('',#1759,.T.);
#360=FACE_BOUND('',#1762,.T.);
#361=FACE_BOUND('',#1764,.T.);
#362=FACE_BOUND('',#1777,.T.);
#363=FACE_BOUND('',#1778,.T.);
#364=FACE_BOUND('',#1780,.T.);
#365=FACE_BOUND('',#1781,.T.);
#366=FACE_BOUND('',#1783,.T.);
#367=FACE_BOUND('',#1785,.T.);
#368=FACE_BOUND('',#1790,.T.);
#369=FACE_BOUND('',#1791,.T.);
#370=FACE_BOUND('',#1792,.T.);
#371=FACE_BOUND('',#1794,.T.);
#372=FACE_BOUND('',#1795,.T.);
#373=FACE_BOUND('',#1796,.T.);
#374=FACE_BOUND('',#1807,.T.);
#375=FACE_BOUND('',#1808,.T.);
#376=FACE_BOUND('',#1809,.T.);
#377=FACE_BOUND('',#1810,.T.);
#378=FACE_BOUND('',#1811,.T.);
#379=FACE_BOUND('',#1812,.T.);
#380=FACE_BOUND('',#1813,.T.);
#381=FACE_BOUND('',#1814,.T.);
#382=FACE_BOUND('',#1815,.T.);
#383=FACE_BOUND('',#1816,.T.);
#384=FACE_BOUND('',#1817,.T.);
#385=FACE_BOUND('',#1818,.T.);
#386=FACE_BOUND('',#1819,.T.);
#387=FACE_BOUND('',#1820,.T.);
#388=FACE_BOUND('',#1821,.T.);
#389=FACE_BOUND('',#1822,.T.);
#390=FACE_BOUND('',#1823,.T.);
#391=FACE_BOUND('',#1824,.T.);
#392=FACE_BOUND('',#1825,.T.);
#393=FACE_BOUND('',#1826,.T.);
#394=FACE_BOUND('',#1827,.T.);
#395=FACE_BOUND('',#1828,.T.);
#396=FACE_BOUND('',#1829,.T.);
#397=FACE_BOUND('',#1830,.T.);
#398=FACE_BOUND('',#1831,.T.);
#399=FACE_BOUND('',#1832,.T.);
#400=FACE_BOUND('',#1833,.T.);
#401=FACE_BOUND('',#1834,.T.);
#402=FACE_BOUND('',#1835,.T.);
#403=FACE_BOUND('',#1836,.T.);
#404=FACE_BOUND('',#1837,.T.);
#405=FACE_BOUND('',#1838,.T.);
#406=FACE_BOUND('',#1839,.T.);
#407=FACE_BOUND('',#1840,.T.);
#408=FACE_BOUND('',#1841,.T.);
#409=FACE_BOUND('',#1842,.T.);
#410=FACE_BOUND('',#1843,.T.);
#411=FACE_BOUND('',#1844,.T.);
#412=FACE_BOUND('',#1845,.T.);
#413=FACE_BOUND('',#1847,.T.);
#414=FACE_BOUND('',#1849,.T.);
#415=FACE_BOUND('',#2053,.T.);
#416=FACE_BOUND('',#2054,.T.);
#417=FACE_BOUND('',#2056,.T.);
#418=FACE_BOUND('',#2057,.T.);
#419=FACE_BOUND('',#2077,.T.);
#420=FACE_BOUND('',#2079,.T.);
#421=FACE_BOUND('',#2085,.T.);
#422=FACE_BOUND('',#2088,.T.);
#423=FACE_BOUND('',#2090,.T.);
#424=FACE_BOUND('',#2100,.T.);
#425=FACE_BOUND('',#2102,.T.);
#426=FACE_BOUND('',#2119,.T.);
#427=FACE_BOUND('',#2125,.T.);
#428=FACE_BOUND('',#2127,.T.);
#429=PLANE('',#10084);
#430=PLANE('',#10085);
#431=PLANE('',#10086);
#432=PLANE('',#10087);
#433=PLANE('',#10088);
#434=PLANE('',#10089);
#435=PLANE('',#10090);
#436=PLANE('',#10091);
#437=PLANE('',#10092);
#438=PLANE('',#10093);
#439=PLANE('',#10094);
#440=PLANE('',#10095);
#441=PLANE('',#10097);
#442=PLANE('',#10098);
#443=PLANE('',#10099);
#444=PLANE('',#10100);
#445=PLANE('',#10101);
#446=PLANE('',#10102);
#447=PLANE('',#10103);
#448=PLANE('',#10104);
#449=PLANE('',#10105);
#450=PLANE('',#10106);
#451=PLANE('',#10107);
#452=PLANE('',#10108);
#453=PLANE('',#10109);
#454=PLANE('',#10110);
#455=PLANE('',#10111);
#456=PLANE('',#10112);
#457=PLANE('',#10113);
#458=PLANE('',#10114);
#459=PLANE('',#10115);
#460=PLANE('',#10116);
#461=PLANE('',#10117);
#462=PLANE('',#10118);
#463=PLANE('',#10119);
#464=PLANE('',#10120);
#465=PLANE('',#10121);
#466=PLANE('',#10122);
#467=PLANE('',#10123);
#468=PLANE('',#10124);
#469=PLANE('',#10125);
#470=PLANE('',#10126);
#471=PLANE('',#10127);
#472=PLANE('',#10128);
#473=PLANE('',#10129);
#474=PLANE('',#10157);
#475=PLANE('',#10158);
#476=PLANE('',#10159);
#477=PLANE('',#10160);
#478=PLANE('',#10161);
#479=PLANE('',#10162);
#480=PLANE('',#10163);
#481=PLANE('',#10164);
#482=PLANE('',#10165);
#483=PLANE('',#10166);
#484=PLANE('',#10167);
#485=PLANE('',#10168);
#486=PLANE('',#10169);
#487=PLANE('',#10170);
#488=PLANE('',#10171);
#489=PLANE('',#10172);
#490=PLANE('',#10173);
#491=PLANE('',#10174);
#492=PLANE('',#10175);
#493=PLANE('',#10176);
#494=PLANE('',#10177);
#495=PLANE('',#10178);
#496=PLANE('',#10179);
#497=PLANE('',#10180);
#498=PLANE('',#10181);
#499=PLANE('',#10182);
#500=PLANE('',#10183);
#501=PLANE('',#10184);
#502=PLANE('',#10185);
#503=PLANE('',#10186);
#504=PLANE('',#10187);
#505=PLANE('',#10188);
#506=PLANE('',#10214);
#507=PLANE('',#10215);
#508=PLANE('',#10216);
#509=PLANE('',#10217);
#510=PLANE('',#10218);
#511=PLANE('',#10219);
#512=PLANE('',#10220);
#513=PLANE('',#10221);
#514=PLANE('',#10222);
#515=PLANE('',#10223);
#516=PLANE('',#10224);
#517=PLANE('',#10225);
#518=PLANE('',#10226);
#519=PLANE('',#10227);
#520=PLANE('',#10228);
#521=PLANE('',#10229);
#522=PLANE('',#10230);
#523=PLANE('',#10231);
#524=PLANE('',#10232);
#525=PLANE('',#10233);
#526=PLANE('',#10234);
#527=PLANE('',#10235);
#528=PLANE('',#10236);
#529=PLANE('',#10237);
#530=PLANE('',#10238);
#531=PLANE('',#10239);
#532=PLANE('',#10240);
#533=PLANE('',#10241);
#534=PLANE('',#10242);
#535=PLANE('',#10243);
#536=PLANE('',#10244);
#537=PLANE('',#10245);
#538=PLANE('',#10246);
#539=PLANE('',#10247);
#540=PLANE('',#10248);
#541=PLANE('',#10249);
#542=PLANE('',#10250);
#543=PLANE('',#10251);
#544=PLANE('',#10252);
#545=PLANE('',#10253);
#546=PLANE('',#10254);
#547=PLANE('',#10255);
#548=PLANE('',#10256);
#549=PLANE('',#10257);
#550=PLANE('',#10258);
#551=PLANE('',#10259);
#552=PLANE('',#10260);
#553=PLANE('',#10261);
#554=PLANE('',#10262);
#555=PLANE('',#10263);
#556=PLANE('',#10264);
#557=PLANE('',#10265);
#558=PLANE('',#10282);
#559=PLANE('',#10283);
#560=PLANE('',#10284);
#561=PLANE('',#10285);
#562=PLANE('',#10286);
#563=PLANE('',#10287);
#564=PLANE('',#10288);
#565=PLANE('',#10289);
#566=PLANE('',#10290);
#567=PLANE('',#10291);
#568=PLANE('',#10292);
#569=PLANE('',#10293);
#570=PLANE('',#10294);
#571=PLANE('',#10295);
#572=PLANE('',#10296);
#573=PLANE('',#10297);
#574=PLANE('',#10298);
#575=PLANE('',#10300);
#576=PLANE('',#10301);
#577=PLANE('',#10302);
#578=PLANE('',#10303);
#579=PLANE('',#10304);
#580=PLANE('',#10305);
#581=PLANE('',#10307);
#582=PLANE('',#10308);
#583=PLANE('',#10309);
#584=PLANE('',#10310);
#585=PLANE('',#10311);
#586=PLANE('',#10312);
#587=PLANE('',#10326);
#588=PLANE('',#10327);
#589=PLANE('',#10328);
#590=PLANE('',#10329);
#591=PLANE('',#10330);
#592=PLANE('',#10331);
#593=PLANE('',#10332);
#594=PLANE('',#10333);
#595=PLANE('',#10350);
#596=PLANE('',#10351);
#597=PLANE('',#10352);
#598=PLANE('',#10353);
#599=PLANE('',#10354);
#600=PLANE('',#10355);
#601=PLANE('',#10372);
#602=PLANE('',#10373);
#603=PLANE('',#10374);
#604=PLANE('',#10375);
#605=PLANE('',#10376);
#606=PLANE('',#10377);
#607=PLANE('',#10396);
#608=PLANE('',#10397);
#609=PLANE('',#10398);
#610=PLANE('',#10399);
#611=PLANE('',#10400);
#612=PLANE('',#10401);
#613=PLANE('',#10402);
#614=PLANE('',#10403);
#615=PLANE('',#10408);
#616=PLANE('',#10409);
#617=PLANE('',#10410);
#618=PLANE('',#10411);
#619=PLANE('',#10412);
#620=PLANE('',#10413);
#621=PLANE('',#10418);
#622=PLANE('',#10419);
#623=PLANE('',#10420);
#624=PLANE('',#10421);
#625=PLANE('',#10422);
#626=PLANE('',#10423);
#627=PLANE('',#10436);
#628=PLANE('',#10437);
#629=PLANE('',#10438);
#630=PLANE('',#10439);
#631=PLANE('',#10444);
#632=PLANE('',#10445);
#633=PLANE('',#10459);
#634=PLANE('',#10460);
#635=PLANE('',#10461);
#636=PLANE('',#10462);
#637=PLANE('',#10463);
#638=PLANE('',#10464);
#639=PLANE('',#10465);
#640=PLANE('',#10466);
#641=PLANE('',#10477);
#642=PLANE('',#10478);
#643=PLANE('',#10479);
#644=PLANE('',#10480);
#645=PLANE('',#10481);
#646=PLANE('',#10482);
#647=PLANE('',#10483);
#648=PLANE('',#10484);
#649=PLANE('',#10485);
#650=PLANE('',#10486);
#651=PLANE('',#10576);
#652=PLANE('',#10577);
#653=PLANE('',#10578);
#654=PLANE('',#10579);
#655=PLANE('',#10580);
#656=PLANE('',#10581);
#657=PLANE('',#10582);
#658=PLANE('',#10583);
#659=PLANE('',#10584);
#660=PLANE('',#10585);
#661=PLANE('',#10586);
#662=PLANE('',#10587);
#663=PLANE('',#10588);
#664=PLANE('',#10589);
#665=PLANE('',#10590);
#666=PLANE('',#10591);
#667=PLANE('',#10592);
#668=PLANE('',#10593);
#669=PLANE('',#10594);
#670=PLANE('',#10595);
#671=PLANE('',#10596);
#672=PLANE('',#10597);
#673=PLANE('',#10598);
#674=PLANE('',#10599);
#675=PLANE('',#10600);
#676=PLANE('',#10601);
#677=PLANE('',#10602);
#678=PLANE('',#10603);
#679=PLANE('',#10604);
#680=PLANE('',#10605);
#681=PLANE('',#10606);
#682=PLANE('',#10607);
#683=PLANE('',#10608);
#684=PLANE('',#10609);
#685=PLANE('',#10610);
#686=PLANE('',#10611);
#687=PLANE('',#10612);
#688=PLANE('',#10613);
#689=PLANE('',#10614);
#690=PLANE('',#10615);
#691=PLANE('',#10616);
#692=PLANE('',#10617);
#693=PLANE('',#10618);
#694=PLANE('',#10619);
#695=PLANE('',#10620);
#696=PLANE('',#10621);
#697=PLANE('',#10622);
#698=PLANE('',#10623);
#699=PLANE('',#10624);
#700=PLANE('',#10625);
#701=PLANE('',#10626);
#702=PLANE('',#10627);
#703=PLANE('',#10628);
#704=PLANE('',#10629);
#705=PLANE('',#10630);
#706=PLANE('',#10631);
#707=PLANE('',#10632);
#708=PLANE('',#10633);
#709=PLANE('',#10634);
#710=PLANE('',#10635);
#711=PLANE('',#10636);
#712=PLANE('',#10637);
#713=PLANE('',#10638);
#714=PLANE('',#10639);
#715=PLANE('',#10640);
#716=PLANE('',#10641);
#717=PLANE('',#10642);
#718=PLANE('',#10643);
#719=PLANE('',#10644);
#720=PLANE('',#10645);
#721=PLANE('',#10646);
#722=PLANE('',#10647);
#723=PLANE('',#10648);
#724=PLANE('',#10649);
#725=PLANE('',#10650);
#726=PLANE('',#10651);
#727=PLANE('',#10652);
#728=PLANE('',#10653);
#729=PLANE('',#10654);
#730=PLANE('',#10655);
#731=PLANE('',#10656);
#732=PLANE('',#10657);
#733=PLANE('',#10658);
#734=PLANE('',#10659);
#735=PLANE('',#10660);
#736=PLANE('',#10661);
#737=PLANE('',#10662);
#738=PLANE('',#10663);
#739=PLANE('',#10664);
#740=PLANE('',#10665);
#741=PLANE('',#10666);
#742=PLANE('',#10667);
#743=PLANE('',#10668);
#744=PLANE('',#10669);
#745=PLANE('',#10670);
#746=PLANE('',#10671);
#747=PLANE('',#10672);
#748=PLANE('',#10673);
#749=PLANE('',#10674);
#750=PLANE('',#10675);
#751=PLANE('',#10676);
#752=PLANE('',#10677);
#753=PLANE('',#10678);
#754=PLANE('',#10679);
#755=PLANE('',#10680);
#756=PLANE('',#10681);
#757=PLANE('',#10682);
#758=PLANE('',#10683);
#759=PLANE('',#10684);
#760=PLANE('',#10685);
#761=PLANE('',#10686);
#762=PLANE('',#10687);
#763=PLANE('',#10688);
#764=PLANE('',#10689);
#765=PLANE('',#10690);
#766=PLANE('',#10691);
#767=PLANE('',#10692);
#768=PLANE('',#10693);
#769=PLANE('',#10694);
#770=PLANE('',#10695);
#771=PLANE('',#10696);
#772=PLANE('',#10697);
#773=PLANE('',#10698);
#774=PLANE('',#10699);
#775=PLANE('',#10700);
#776=PLANE('',#10701);
#777=PLANE('',#10702);
#778=PLANE('',#10703);
#779=PLANE('',#10704);
#780=PLANE('',#10705);
#781=PLANE('',#10706);
#782=PLANE('',#10707);
#783=PLANE('',#10708);
#784=PLANE('',#10709);
#785=PLANE('',#10710);
#786=PLANE('',#10711);
#787=PLANE('',#10712);
#788=PLANE('',#10713);
#789=PLANE('',#10714);
#790=PLANE('',#10715);
#791=PLANE('',#10716);
#792=PLANE('',#10717);
#793=PLANE('',#10718);
#794=PLANE('',#10719);
#795=PLANE('',#10720);
#796=PLANE('',#10721);
#797=PLANE('',#10722);
#798=PLANE('',#10723);
#799=PLANE('',#10724);
#800=PLANE('',#10725);
#801=PLANE('',#10726);
#802=PLANE('',#10727);
#803=PLANE('',#10728);
#804=PLANE('',#10729);
#805=PLANE('',#10730);
#806=PLANE('',#10731);
#807=PLANE('',#10732);
#808=PLANE('',#10733);
#809=PLANE('',#10734);
#810=PLANE('',#10735);
#811=PLANE('',#10736);
#812=PLANE('',#10737);
#813=PLANE('',#10738);
#814=PLANE('',#10739);
#815=PLANE('',#10740);
#816=PLANE('',#10741);
#817=PLANE('',#10742);
#818=PLANE('',#10743);
#819=PLANE('',#10744);
#820=PLANE('',#10745);
#821=PLANE('',#10746);
#822=PLANE('',#10747);
#823=PLANE('',#10748);
#824=PLANE('',#10749);
#825=PLANE('',#10750);
#826=PLANE('',#10751);
#827=PLANE('',#10752);
#828=PLANE('',#10753);
#829=PLANE('',#10754);
#830=PLANE('',#10755);
#831=PLANE('',#10756);
#832=PLANE('',#10757);
#833=PLANE('',#10758);
#834=PLANE('',#10759);
#835=PLANE('',#10760);
#836=PLANE('',#10761);
#837=PLANE('',#10762);
#838=PLANE('',#10763);
#839=PLANE('',#10764);
#840=PLANE('',#10765);
#841=PLANE('',#10766);
#842=PLANE('',#10767);
#843=PLANE('',#10768);
#844=PLANE('',#10769);
#845=PLANE('',#10770);
#846=PLANE('',#10771);
#847=PLANE('',#10772);
#848=PLANE('',#10773);
#849=PLANE('',#10774);
#850=PLANE('',#10775);
#851=PLANE('',#10776);
#852=PLANE('',#10777);
#853=PLANE('',#10785);
#854=PLANE('',#10786);
#855=PLANE('',#10787);
#856=PLANE('',#10788);
#857=PLANE('',#10789);
#858=PLANE('',#10790);
#859=PLANE('',#10791);
#860=PLANE('',#10792);
#861=PLANE('',#10793);
#862=PLANE('',#10794);
#863=PLANE('',#10795);
#864=PLANE('',#10796);
#865=PLANE('',#10797);
#866=PLANE('',#10798);
#867=PLANE('',#10799);
#868=PLANE('',#10800);
#869=PLANE('',#10813);
#870=PLANE('',#10814);
#871=PLANE('',#10822);
#872=PLANE('',#10823);
#873=PLANE('',#10824);
#874=PLANE('',#10829);
#875=PLANE('',#10830);
#876=PLANE('',#10831);
#877=PLANE('',#10832);
#878=PLANE('',#10833);
#879=PLANE('',#10834);
#880=PLANE('',#10835);
#881=PLANE('',#10836);
#882=PLANE('',#10844);
#883=PLANE('',#10845);
#884=PLANE('',#10846);
#885=PLANE('',#10847);
#886=PLANE('',#10848);
#887=PLANE('',#10849);
#888=PLANE('',#10850);
#889=PLANE('',#10851);
#890=PLANE('',#10852);
#891=PLANE('',#10853);
#892=PLANE('',#10858);
#893=PLANE('',#10859);
#894=PLANE('',#10860);
#895=PLANE('',#10861);
#896=PLANE('',#10862);
#897=PLANE('',#10863);
#898=PLANE('',#10864);
#899=PLANE('',#10865);
#900=PLANE('',#10866);
#901=PLANE('',#10874);
#902=PLANE('',#10875);
#903=PLANE('',#10876);
#904=PLANE('',#10877);
#905=PLANE('',#10878);
#906=PLANE('',#10879);
#907=PLANE('',#10880);
#908=PLANE('',#10881);
#909=PLANE('',#10882);
#910=PLANE('',#10883);
#911=FACE_OUTER_BOUND('',#1462,.T.);
#912=FACE_OUTER_BOUND('',#1463,.T.);
#913=FACE_OUTER_BOUND('',#1464,.T.);
#914=FACE_OUTER_BOUND('',#1467,.T.);
#915=FACE_OUTER_BOUND('',#1468,.T.);
#916=FACE_OUTER_BOUND('',#1469,.T.);
#917=FACE_OUTER_BOUND('',#1470,.T.);
#918=FACE_OUTER_BOUND('',#1471,.T.);
#919=FACE_OUTER_BOUND('',#1472,.T.);
#920=FACE_OUTER_BOUND('',#1473,.T.);
#921=FACE_OUTER_BOUND('',#1474,.T.);
#922=FACE_OUTER_BOUND('',#1475,.T.);
#923=FACE_OUTER_BOUND('',#1476,.T.);
#924=FACE_OUTER_BOUND('',#1477,.T.);
#925=FACE_OUTER_BOUND('',#1478,.T.);
#926=FACE_OUTER_BOUND('',#1479,.T.);
#927=FACE_OUTER_BOUND('',#1480,.T.);
#928=FACE_OUTER_BOUND('',#1481,.T.);
#929=FACE_OUTER_BOUND('',#1482,.T.);
#930=FACE_OUTER_BOUND('',#1483,.T.);
#931=FACE_OUTER_BOUND('',#1485,.T.);
#932=FACE_OUTER_BOUND('',#1486,.T.);
#933=FACE_OUTER_BOUND('',#1487,.T.);
#934=FACE_OUTER_BOUND('',#1488,.T.);
#935=FACE_OUTER_BOUND('',#1489,.T.);
#936=FACE_OUTER_BOUND('',#1490,.T.);
#937=FACE_OUTER_BOUND('',#1492,.T.);
#938=FACE_OUTER_BOUND('',#1493,.T.);
#939=FACE_OUTER_BOUND('',#1494,.T.);
#940=FACE_OUTER_BOUND('',#1495,.T.);
#941=FACE_OUTER_BOUND('',#1496,.T.);
#942=FACE_OUTER_BOUND('',#1497,.T.);
#943=FACE_OUTER_BOUND('',#1498,.T.);
#944=FACE_OUTER_BOUND('',#1499,.T.);
#945=FACE_OUTER_BOUND('',#1500,.T.);
#946=FACE_OUTER_BOUND('',#1501,.T.);
#947=FACE_OUTER_BOUND('',#1502,.T.);
#948=FACE_OUTER_BOUND('',#1503,.T.);
#949=FACE_OUTER_BOUND('',#1504,.T.);
#950=FACE_OUTER_BOUND('',#1505,.T.);
#951=FACE_OUTER_BOUND('',#1506,.T.);
#952=FACE_OUTER_BOUND('',#1507,.T.);
#953=FACE_OUTER_BOUND('',#1508,.T.);
#954=FACE_OUTER_BOUND('',#1509,.T.);
#955=FACE_OUTER_BOUND('',#1510,.T.);
#956=FACE_OUTER_BOUND('',#1511,.T.);
#957=FACE_OUTER_BOUND('',#1512,.T.);
#958=FACE_OUTER_BOUND('',#1513,.T.);
#959=FACE_OUTER_BOUND('',#1514,.T.);
#960=FACE_OUTER_BOUND('',#1515,.T.);
#961=FACE_OUTER_BOUND('',#1516,.T.);
#962=FACE_OUTER_BOUND('',#1517,.T.);
#963=FACE_OUTER_BOUND('',#1518,.T.);
#964=FACE_OUTER_BOUND('',#1519,.T.);
#965=FACE_OUTER_BOUND('',#1520,.T.);
#966=FACE_OUTER_BOUND('',#1523,.T.);
#967=FACE_OUTER_BOUND('',#1527,.T.);
#968=FACE_OUTER_BOUND('',#1528,.T.);
#969=FACE_OUTER_BOUND('',#1529,.T.);
#970=FACE_OUTER_BOUND('',#1530,.T.);
#971=FACE_OUTER_BOUND('',#1531,.T.);
#972=FACE_OUTER_BOUND('',#1532,.T.);
#973=FACE_OUTER_BOUND('',#1533,.T.);
#974=FACE_OUTER_BOUND('',#1534,.T.);
#975=FACE_OUTER_BOUND('',#1538,.T.);
#976=FACE_OUTER_BOUND('',#1539,.T.);
#977=FACE_OUTER_BOUND('',#1540,.T.);
#978=FACE_OUTER_BOUND('',#1541,.T.);
#979=FACE_OUTER_BOUND('',#1542,.T.);
#980=FACE_OUTER_BOUND('',#1543,.T.);
#981=FACE_OUTER_BOUND('',#1544,.T.);
#982=FACE_OUTER_BOUND('',#1545,.T.);
#983=FACE_OUTER_BOUND('',#1546,.T.);
#984=FACE_OUTER_BOUND('',#1548,.T.);
#985=FACE_OUTER_BOUND('',#1549,.T.);
#986=FACE_OUTER_BOUND('',#1550,.T.);
#987=FACE_OUTER_BOUND('',#1551,.T.);
#988=FACE_OUTER_BOUND('',#1552,.T.);
#989=FACE_OUTER_BOUND('',#1553,.T.);
#990=FACE_OUTER_BOUND('',#1555,.T.);
#991=FACE_OUTER_BOUND('',#1556,.T.);
#992=FACE_OUTER_BOUND('',#1557,.T.);
#993=FACE_OUTER_BOUND('',#1558,.T.);
#994=FACE_OUTER_BOUND('',#1559,.T.);
#995=FACE_OUTER_BOUND('',#1560,.T.);
#996=FACE_OUTER_BOUND('',#1561,.T.);
#997=FACE_OUTER_BOUND('',#1562,.T.);
#998=FACE_OUTER_BOUND('',#1563,.T.);
#999=FACE_OUTER_BOUND('',#1564,.T.);
#1000=FACE_OUTER_BOUND('',#1565,.T.);
#1001=FACE_OUTER_BOUND('',#1566,.T.);
#1002=FACE_OUTER_BOUND('',#1567,.T.);
#1003=FACE_OUTER_BOUND('',#1568,.T.);
#1004=FACE_OUTER_BOUND('',#1570,.T.);
#1005=FACE_OUTER_BOUND('',#1571,.T.);
#1006=FACE_OUTER_BOUND('',#1572,.T.);
#1007=FACE_OUTER_BOUND('',#1573,.T.);
#1008=FACE_OUTER_BOUND('',#1574,.T.);
#1009=FACE_OUTER_BOUND('',#1575,.T.);
#1010=FACE_OUTER_BOUND('',#1576,.T.);
#1011=FACE_OUTER_BOUND('',#1577,.T.);
#1012=FACE_OUTER_BOUND('',#1578,.T.);
#1013=FACE_OUTER_BOUND('',#1579,.T.);
#1014=FACE_OUTER_BOUND('',#1580,.T.);
#1015=FACE_OUTER_BOUND('',#1581,.T.);
#1016=FACE_OUTER_BOUND('',#1582,.T.);
#1017=FACE_OUTER_BOUND('',#1586,.T.);
#1018=FACE_OUTER_BOUND('',#1590,.T.);
#1019=FACE_OUTER_BOUND('',#1591,.T.);
#1020=FACE_OUTER_BOUND('',#1592,.T.);
#1021=FACE_OUTER_BOUND('',#1593,.T.);
#1022=FACE_OUTER_BOUND('',#1594,.T.);
#1023=FACE_OUTER_BOUND('',#1595,.T.);
#1024=FACE_OUTER_BOUND('',#1596,.T.);
#1025=FACE_OUTER_BOUND('',#1598,.T.);
#1026=FACE_OUTER_BOUND('',#1599,.T.);
#1027=FACE_OUTER_BOUND('',#1600,.T.);
#1028=FACE_OUTER_BOUND('',#1601,.T.);
#1029=FACE_OUTER_BOUND('',#1602,.T.);
#1030=FACE_OUTER_BOUND('',#1603,.T.);
#1031=FACE_OUTER_BOUND('',#1604,.T.);
#1032=FACE_OUTER_BOUND('',#1605,.T.);
#1033=FACE_OUTER_BOUND('',#1608,.T.);
#1034=FACE_OUTER_BOUND('',#1609,.T.);
#1035=FACE_OUTER_BOUND('',#1610,.T.);
#1036=FACE_OUTER_BOUND('',#1611,.T.);
#1037=FACE_OUTER_BOUND('',#1612,.T.);
#1038=FACE_OUTER_BOUND('',#1613,.T.);
#1039=FACE_OUTER_BOUND('',#1615,.T.);
#1040=FACE_OUTER_BOUND('',#1616,.T.);
#1041=FACE_OUTER_BOUND('',#1617,.T.);
#1042=FACE_OUTER_BOUND('',#1618,.T.);
#1043=FACE_OUTER_BOUND('',#1619,.T.);
#1044=FACE_OUTER_BOUND('',#1620,.T.);
#1045=FACE_OUTER_BOUND('',#1621,.T.);
#1046=FACE_OUTER_BOUND('',#1622,.T.);
#1047=FACE_OUTER_BOUND('',#1623,.T.);
#1048=FACE_OUTER_BOUND('',#1624,.T.);
#1049=FACE_OUTER_BOUND('',#1625,.T.);
#1050=FACE_OUTER_BOUND('',#1626,.T.);
#1051=FACE_OUTER_BOUND('',#1627,.T.);
#1052=FACE_OUTER_BOUND('',#1628,.T.);
#1053=FACE_OUTER_BOUND('',#1629,.T.);
#1054=FACE_OUTER_BOUND('',#1630,.T.);
#1055=FACE_OUTER_BOUND('',#1631,.T.);
#1056=FACE_OUTER_BOUND('',#1632,.T.);
#1057=FACE_OUTER_BOUND('',#1633,.T.);
#1058=FACE_OUTER_BOUND('',#1634,.T.);
#1059=FACE_OUTER_BOUND('',#1635,.T.);
#1060=FACE_OUTER_BOUND('',#1636,.T.);
#1061=FACE_OUTER_BOUND('',#1637,.T.);
#1062=FACE_OUTER_BOUND('',#1638,.T.);
#1063=FACE_OUTER_BOUND('',#1639,.T.);
#1064=FACE_OUTER_BOUND('',#1640,.T.);
#1065=FACE_OUTER_BOUND('',#1641,.T.);
#1066=FACE_OUTER_BOUND('',#1642,.T.);
#1067=FACE_OUTER_BOUND('',#1643,.T.);
#1068=FACE_OUTER_BOUND('',#1646,.T.);
#1069=FACE_OUTER_BOUND('',#1648,.T.);
#1070=FACE_OUTER_BOUND('',#1649,.T.);
#1071=FACE_OUTER_BOUND('',#1650,.T.);
#1072=FACE_OUTER_BOUND('',#1653,.T.);
#1073=FACE_OUTER_BOUND('',#1654,.T.);
#1074=FACE_OUTER_BOUND('',#1655,.T.);
#1075=FACE_OUTER_BOUND('',#1656,.T.);
#1076=FACE_OUTER_BOUND('',#1657,.T.);
#1077=FACE_OUTER_BOUND('',#1658,.T.);
#1078=FACE_OUTER_BOUND('',#1659,.T.);
#1079=FACE_OUTER_BOUND('',#1660,.T.);
#1080=FACE_OUTER_BOUND('',#1661,.T.);
#1081=FACE_OUTER_BOUND('',#1662,.T.);
#1082=FACE_OUTER_BOUND('',#1663,.T.);
#1083=FACE_OUTER_BOUND('',#1664,.T.);
#1084=FACE_OUTER_BOUND('',#1665,.T.);
#1085=FACE_OUTER_BOUND('',#1666,.T.);
#1086=FACE_OUTER_BOUND('',#1667,.T.);
#1087=FACE_OUTER_BOUND('',#1668,.T.);
#1088=FACE_OUTER_BOUND('',#1669,.T.);
#1089=FACE_OUTER_BOUND('',#1670,.T.);
#1090=FACE_OUTER_BOUND('',#1671,.T.);
#1091=FACE_OUTER_BOUND('',#1672,.T.);
#1092=FACE_OUTER_BOUND('',#1673,.T.);
#1093=FACE_OUTER_BOUND('',#1674,.T.);
#1094=FACE_OUTER_BOUND('',#1675,.T.);
#1095=FACE_OUTER_BOUND('',#1676,.T.);
#1096=FACE_OUTER_BOUND('',#1677,.T.);
#1097=FACE_OUTER_BOUND('',#1678,.T.);
#1098=FACE_OUTER_BOUND('',#1681,.T.);
#1099=FACE_OUTER_BOUND('',#1684,.T.);
#1100=FACE_OUTER_BOUND('',#1686,.T.);
#1101=FACE_OUTER_BOUND('',#1688,.T.);
#1102=FACE_OUTER_BOUND('',#1689,.T.);
#1103=FACE_OUTER_BOUND('',#1690,.T.);
#1104=FACE_OUTER_BOUND('',#1691,.T.);
#1105=FACE_OUTER_BOUND('',#1692,.T.);
#1106=FACE_OUTER_BOUND('',#1693,.T.);
#1107=FACE_OUTER_BOUND('',#1694,.T.);
#1108=FACE_OUTER_BOUND('',#1696,.T.);
#1109=FACE_OUTER_BOUND('',#1698,.T.);
#1110=FACE_OUTER_BOUND('',#1700,.T.);
#1111=FACE_OUTER_BOUND('',#1702,.T.);
#1112=FACE_OUTER_BOUND('',#1703,.T.);
#1113=FACE_OUTER_BOUND('',#1704,.T.);
#1114=FACE_OUTER_BOUND('',#1705,.T.);
#1115=FACE_OUTER_BOUND('',#1706,.T.);
#1116=FACE_OUTER_BOUND('',#1707,.T.);
#1117=FACE_OUTER_BOUND('',#1708,.T.);
#1118=FACE_OUTER_BOUND('',#1709,.T.);
#1119=FACE_OUTER_BOUND('',#1711,.T.);
#1120=FACE_OUTER_BOUND('',#1713,.T.);
#1121=FACE_OUTER_BOUND('',#1715,.T.);
#1122=FACE_OUTER_BOUND('',#1717,.T.);
#1123=FACE_OUTER_BOUND('',#1718,.T.);
#1124=FACE_OUTER_BOUND('',#1719,.T.);
#1125=FACE_OUTER_BOUND('',#1720,.T.);
#1126=FACE_OUTER_BOUND('',#1721,.T.);
#1127=FACE_OUTER_BOUND('',#1722,.T.);
#1128=FACE_OUTER_BOUND('',#1724,.T.);
#1129=FACE_OUTER_BOUND('',#1725,.T.);
#1130=FACE_OUTER_BOUND('',#1726,.T.);
#1131=FACE_OUTER_BOUND('',#1728,.T.);
#1132=FACE_OUTER_BOUND('',#1730,.T.);
#1133=FACE_OUTER_BOUND('',#1731,.T.);
#1134=FACE_OUTER_BOUND('',#1733,.T.);
#1135=FACE_OUTER_BOUND('',#1735,.T.);
#1136=FACE_OUTER_BOUND('',#1736,.T.);
#1137=FACE_OUTER_BOUND('',#1737,.T.);
#1138=FACE_OUTER_BOUND('',#1739,.T.);
#1139=FACE_OUTER_BOUND('',#1741,.T.);
#1140=FACE_OUTER_BOUND('',#1742,.T.);
#1141=FACE_OUTER_BOUND('',#1743,.T.);
#1142=FACE_OUTER_BOUND('',#1744,.T.);
#1143=FACE_OUTER_BOUND('',#1745,.T.);
#1144=FACE_OUTER_BOUND('',#1746,.T.);
#1145=FACE_OUTER_BOUND('',#1748,.T.);
#1146=FACE_OUTER_BOUND('',#1750,.T.);
#1147=FACE_OUTER_BOUND('',#1751,.T.);
#1148=FACE_OUTER_BOUND('',#1752,.T.);
#1149=FACE_OUTER_BOUND('',#1753,.T.);
#1150=FACE_OUTER_BOUND('',#1754,.T.);
#1151=FACE_OUTER_BOUND('',#1755,.T.);
#1152=FACE_OUTER_BOUND('',#1756,.T.);
#1153=FACE_OUTER_BOUND('',#1757,.T.);
#1154=FACE_OUTER_BOUND('',#1758,.T.);
#1155=FACE_OUTER_BOUND('',#1760,.T.);
#1156=FACE_OUTER_BOUND('',#1761,.T.);
#1157=FACE_OUTER_BOUND('',#1763,.T.);
#1158=FACE_OUTER_BOUND('',#1765,.T.);
#1159=FACE_OUTER_BOUND('',#1766,.T.);
#1160=FACE_OUTER_BOUND('',#1767,.T.);
#1161=FACE_OUTER_BOUND('',#1768,.T.);
#1162=FACE_OUTER_BOUND('',#1769,.T.);
#1163=FACE_OUTER_BOUND('',#1770,.T.);
#1164=FACE_OUTER_BOUND('',#1771,.T.);
#1165=FACE_OUTER_BOUND('',#1772,.T.);
#1166=FACE_OUTER_BOUND('',#1773,.T.);
#1167=FACE_OUTER_BOUND('',#1774,.T.);
#1168=FACE_OUTER_BOUND('',#1775,.T.);
#1169=FACE_OUTER_BOUND('',#1776,.T.);
#1170=FACE_OUTER_BOUND('',#1779,.T.);
#1171=FACE_OUTER_BOUND('',#1782,.T.);
#1172=FACE_OUTER_BOUND('',#1784,.T.);
#1173=FACE_OUTER_BOUND('',#1786,.T.);
#1174=FACE_OUTER_BOUND('',#1787,.T.);
#1175=FACE_OUTER_BOUND('',#1788,.T.);
#1176=FACE_OUTER_BOUND('',#1789,.T.);
#1177=FACE_OUTER_BOUND('',#1793,.T.);
#1178=FACE_OUTER_BOUND('',#1797,.T.);
#1179=FACE_OUTER_BOUND('',#1798,.T.);
#1180=FACE_OUTER_BOUND('',#1799,.T.);
#1181=FACE_OUTER_BOUND('',#1800,.T.);
#1182=FACE_OUTER_BOUND('',#1801,.T.);
#1183=FACE_OUTER_BOUND('',#1802,.T.);
#1184=FACE_OUTER_BOUND('',#1803,.T.);
#1185=FACE_OUTER_BOUND('',#1804,.T.);
#1186=FACE_OUTER_BOUND('',#1805,.T.);
#1187=FACE_OUTER_BOUND('',#1806,.T.);
#1188=FACE_OUTER_BOUND('',#1846,.T.);
#1189=FACE_OUTER_BOUND('',#1848,.T.);
#1190=FACE_OUTER_BOUND('',#1850,.T.);
#1191=FACE_OUTER_BOUND('',#1851,.T.);
#1192=FACE_OUTER_BOUND('',#1852,.T.);
#1193=FACE_OUTER_BOUND('',#1853,.T.);
#1194=FACE_OUTER_BOUND('',#1854,.T.);
#1195=FACE_OUTER_BOUND('',#1855,.T.);
#1196=FACE_OUTER_BOUND('',#1856,.T.);
#1197=FACE_OUTER_BOUND('',#1857,.T.);
#1198=FACE_OUTER_BOUND('',#1858,.T.);
#1199=FACE_OUTER_BOUND('',#1859,.T.);
#1200=FACE_OUTER_BOUND('',#1860,.T.);
#1201=FACE_OUTER_BOUND('',#1861,.T.);
#1202=FACE_OUTER_BOUND('',#1862,.T.);
#1203=FACE_OUTER_BOUND('',#1863,.T.);
#1204=FACE_OUTER_BOUND('',#1864,.T.);
#1205=FACE_OUTER_BOUND('',#1865,.T.);
#1206=FACE_OUTER_BOUND('',#1866,.T.);
#1207=FACE_OUTER_BOUND('',#1867,.T.);
#1208=FACE_OUTER_BOUND('',#1868,.T.);
#1209=FACE_OUTER_BOUND('',#1869,.T.);
#1210=FACE_OUTER_BOUND('',#1870,.T.);
#1211=FACE_OUTER_BOUND('',#1871,.T.);
#1212=FACE_OUTER_BOUND('',#1872,.T.);
#1213=FACE_OUTER_BOUND('',#1873,.T.);
#1214=FACE_OUTER_BOUND('',#1874,.T.);
#1215=FACE_OUTER_BOUND('',#1875,.T.);
#1216=FACE_OUTER_BOUND('',#1876,.T.);
#1217=FACE_OUTER_BOUND('',#1877,.T.);
#1218=FACE_OUTER_BOUND('',#1878,.T.);
#1219=FACE_OUTER_BOUND('',#1879,.T.);
#1220=FACE_OUTER_BOUND('',#1880,.T.);
#1221=FACE_OUTER_BOUND('',#1881,.T.);
#1222=FACE_OUTER_BOUND('',#1882,.T.);
#1223=FACE_OUTER_BOUND('',#1883,.T.);
#1224=FACE_OUTER_BOUND('',#1884,.T.);
#1225=FACE_OUTER_BOUND('',#1885,.T.);
#1226=FACE_OUTER_BOUND('',#1886,.T.);
#1227=FACE_OUTER_BOUND('',#1887,.T.);
#1228=FACE_OUTER_BOUND('',#1888,.T.);
#1229=FACE_OUTER_BOUND('',#1889,.T.);
#1230=FACE_OUTER_BOUND('',#1890,.T.);
#1231=FACE_OUTER_BOUND('',#1891,.T.);
#1232=FACE_OUTER_BOUND('',#1892,.T.);
#1233=FACE_OUTER_BOUND('',#1893,.T.);
#1234=FACE_OUTER_BOUND('',#1894,.T.);
#1235=FACE_OUTER_BOUND('',#1895,.T.);
#1236=FACE_OUTER_BOUND('',#1896,.T.);
#1237=FACE_OUTER_BOUND('',#1897,.T.);
#1238=FACE_OUTER_BOUND('',#1898,.T.);
#1239=FACE_OUTER_BOUND('',#1899,.T.);
#1240=FACE_OUTER_BOUND('',#1900,.T.);
#1241=FACE_OUTER_BOUND('',#1901,.T.);
#1242=FACE_OUTER_BOUND('',#1902,.T.);
#1243=FACE_OUTER_BOUND('',#1903,.T.);
#1244=FACE_OUTER_BOUND('',#1904,.T.);
#1245=FACE_OUTER_BOUND('',#1905,.T.);
#1246=FACE_OUTER_BOUND('',#1906,.T.);
#1247=FACE_OUTER_BOUND('',#1907,.T.);
#1248=FACE_OUTER_BOUND('',#1908,.T.);
#1249=FACE_OUTER_BOUND('',#1909,.T.);
#1250=FACE_OUTER_BOUND('',#1910,.T.);
#1251=FACE_OUTER_BOUND('',#1911,.T.);
#1252=FACE_OUTER_BOUND('',#1912,.T.);
#1253=FACE_OUTER_BOUND('',#1913,.T.);
#1254=FACE_OUTER_BOUND('',#1914,.T.);
#1255=FACE_OUTER_BOUND('',#1915,.T.);
#1256=FACE_OUTER_BOUND('',#1916,.T.);
#1257=FACE_OUTER_BOUND('',#1917,.T.);
#1258=FACE_OUTER_BOUND('',#1918,.T.);
#1259=FACE_OUTER_BOUND('',#1919,.T.);
#1260=FACE_OUTER_BOUND('',#1920,.T.);
#1261=FACE_OUTER_BOUND('',#1921,.T.);
#1262=FACE_OUTER_BOUND('',#1922,.T.);
#1263=FACE_OUTER_BOUND('',#1923,.T.);
#1264=FACE_OUTER_BOUND('',#1924,.T.);
#1265=FACE_OUTER_BOUND('',#1925,.T.);
#1266=FACE_OUTER_BOUND('',#1926,.T.);
#1267=FACE_OUTER_BOUND('',#1927,.T.);
#1268=FACE_OUTER_BOUND('',#1928,.T.);
#1269=FACE_OUTER_BOUND('',#1929,.T.);
#1270=FACE_OUTER_BOUND('',#1930,.T.);
#1271=FACE_OUTER_BOUND('',#1931,.T.);
#1272=FACE_OUTER_BOUND('',#1932,.T.);
#1273=FACE_OUTER_BOUND('',#1933,.T.);
#1274=FACE_OUTER_BOUND('',#1934,.T.);
#1275=FACE_OUTER_BOUND('',#1935,.T.);
#1276=FACE_OUTER_BOUND('',#1936,.T.);
#1277=FACE_OUTER_BOUND('',#1937,.T.);
#1278=FACE_OUTER_BOUND('',#1938,.T.);
#1279=FACE_OUTER_BOUND('',#1939,.T.);
#1280=FACE_OUTER_BOUND('',#1940,.T.);
#1281=FACE_OUTER_BOUND('',#1941,.T.);
#1282=FACE_OUTER_BOUND('',#1942,.T.);
#1283=FACE_OUTER_BOUND('',#1943,.T.);
#1284=FACE_OUTER_BOUND('',#1944,.T.);
#1285=FACE_OUTER_BOUND('',#1945,.T.);
#1286=FACE_OUTER_BOUND('',#1946,.T.);
#1287=FACE_OUTER_BOUND('',#1947,.T.);
#1288=FACE_OUTER_BOUND('',#1948,.T.);
#1289=FACE_OUTER_BOUND('',#1949,.T.);
#1290=FACE_OUTER_BOUND('',#1950,.T.);
#1291=FACE_OUTER_BOUND('',#1951,.T.);
#1292=FACE_OUTER_BOUND('',#1952,.T.);
#1293=FACE_OUTER_BOUND('',#1953,.T.);
#1294=FACE_OUTER_BOUND('',#1954,.T.);
#1295=FACE_OUTER_BOUND('',#1955,.T.);
#1296=FACE_OUTER_BOUND('',#1956,.T.);
#1297=FACE_OUTER_BOUND('',#1957,.T.);
#1298=FACE_OUTER_BOUND('',#1958,.T.);
#1299=FACE_OUTER_BOUND('',#1959,.T.);
#1300=FACE_OUTER_BOUND('',#1960,.T.);
#1301=FACE_OUTER_BOUND('',#1961,.T.);
#1302=FACE_OUTER_BOUND('',#1962,.T.);
#1303=FACE_OUTER_BOUND('',#1963,.T.);
#1304=FACE_OUTER_BOUND('',#1964,.T.);
#1305=FACE_OUTER_BOUND('',#1965,.T.);
#1306=FACE_OUTER_BOUND('',#1966,.T.);
#1307=FACE_OUTER_BOUND('',#1967,.T.);
#1308=FACE_OUTER_BOUND('',#1968,.T.);
#1309=FACE_OUTER_BOUND('',#1969,.T.);
#1310=FACE_OUTER_BOUND('',#1970,.T.);
#1311=FACE_OUTER_BOUND('',#1971,.T.);
#1312=FACE_OUTER_BOUND('',#1972,.T.);
#1313=FACE_OUTER_BOUND('',#1973,.T.);
#1314=FACE_OUTER_BOUND('',#1974,.T.);
#1315=FACE_OUTER_BOUND('',#1975,.T.);
#1316=FACE_OUTER_BOUND('',#1976,.T.);
#1317=FACE_OUTER_BOUND('',#1977,.T.);
#1318=FACE_OUTER_BOUND('',#1978,.T.);
#1319=FACE_OUTER_BOUND('',#1979,.T.);
#1320=FACE_OUTER_BOUND('',#1980,.T.);
#1321=FACE_OUTER_BOUND('',#1981,.T.);
#1322=FACE_OUTER_BOUND('',#1982,.T.);
#1323=FACE_OUTER_BOUND('',#1983,.T.);
#1324=FACE_OUTER_BOUND('',#1984,.T.);
#1325=FACE_OUTER_BOUND('',#1985,.T.);
#1326=FACE_OUTER_BOUND('',#1986,.T.);
#1327=FACE_OUTER_BOUND('',#1987,.T.);
#1328=FACE_OUTER_BOUND('',#1988,.T.);
#1329=FACE_OUTER_BOUND('',#1989,.T.);
#1330=FACE_OUTER_BOUND('',#1990,.T.);
#1331=FACE_OUTER_BOUND('',#1991,.T.);
#1332=FACE_OUTER_BOUND('',#1992,.T.);
#1333=FACE_OUTER_BOUND('',#1993,.T.);
#1334=FACE_OUTER_BOUND('',#1994,.T.);
#1335=FACE_OUTER_BOUND('',#1995,.T.);
#1336=FACE_OUTER_BOUND('',#1996,.T.);
#1337=FACE_OUTER_BOUND('',#1997,.T.);
#1338=FACE_OUTER_BOUND('',#1998,.T.);
#1339=FACE_OUTER_BOUND('',#1999,.T.);
#1340=FACE_OUTER_BOUND('',#2000,.T.);
#1341=FACE_OUTER_BOUND('',#2001,.T.);
#1342=FACE_OUTER_BOUND('',#2002,.T.);
#1343=FACE_OUTER_BOUND('',#2003,.T.);
#1344=FACE_OUTER_BOUND('',#2004,.T.);
#1345=FACE_OUTER_BOUND('',#2005,.T.);
#1346=FACE_OUTER_BOUND('',#2006,.T.);
#1347=FACE_OUTER_BOUND('',#2007,.T.);
#1348=FACE_OUTER_BOUND('',#2008,.T.);
#1349=FACE_OUTER_BOUND('',#2009,.T.);
#1350=FACE_OUTER_BOUND('',#2010,.T.);
#1351=FACE_OUTER_BOUND('',#2011,.T.);
#1352=FACE_OUTER_BOUND('',#2012,.T.);
#1353=FACE_OUTER_BOUND('',#2013,.T.);
#1354=FACE_OUTER_BOUND('',#2014,.T.);
#1355=FACE_OUTER_BOUND('',#2015,.T.);
#1356=FACE_OUTER_BOUND('',#2016,.T.);
#1357=FACE_OUTER_BOUND('',#2017,.T.);
#1358=FACE_OUTER_BOUND('',#2018,.T.);
#1359=FACE_OUTER_BOUND('',#2019,.T.);
#1360=FACE_OUTER_BOUND('',#2020,.T.);
#1361=FACE_OUTER_BOUND('',#2021,.T.);
#1362=FACE_OUTER_BOUND('',#2022,.T.);
#1363=FACE_OUTER_BOUND('',#2023,.T.);
#1364=FACE_OUTER_BOUND('',#2024,.T.);
#1365=FACE_OUTER_BOUND('',#2025,.T.);
#1366=FACE_OUTER_BOUND('',#2026,.T.);
#1367=FACE_OUTER_BOUND('',#2027,.T.);
#1368=FACE_OUTER_BOUND('',#2028,.T.);
#1369=FACE_OUTER_BOUND('',#2029,.T.);
#1370=FACE_OUTER_BOUND('',#2030,.T.);
#1371=FACE_OUTER_BOUND('',#2031,.T.);
#1372=FACE_OUTER_BOUND('',#2032,.T.);
#1373=FACE_OUTER_BOUND('',#2033,.T.);
#1374=FACE_OUTER_BOUND('',#2034,.T.);
#1375=FACE_OUTER_BOUND('',#2035,.T.);
#1376=FACE_OUTER_BOUND('',#2036,.T.);
#1377=FACE_OUTER_BOUND('',#2037,.T.);
#1378=FACE_OUTER_BOUND('',#2038,.T.);
#1379=FACE_OUTER_BOUND('',#2039,.T.);
#1380=FACE_OUTER_BOUND('',#2040,.T.);
#1381=FACE_OUTER_BOUND('',#2041,.T.);
#1382=FACE_OUTER_BOUND('',#2042,.T.);
#1383=FACE_OUTER_BOUND('',#2043,.T.);
#1384=FACE_OUTER_BOUND('',#2044,.T.);
#1385=FACE_OUTER_BOUND('',#2045,.T.);
#1386=FACE_OUTER_BOUND('',#2046,.T.);
#1387=FACE_OUTER_BOUND('',#2047,.T.);
#1388=FACE_OUTER_BOUND('',#2048,.T.);
#1389=FACE_OUTER_BOUND('',#2049,.T.);
#1390=FACE_OUTER_BOUND('',#2050,.T.);
#1391=FACE_OUTER_BOUND('',#2051,.T.);
#1392=FACE_OUTER_BOUND('',#2052,.T.);
#1393=FACE_OUTER_BOUND('',#2055,.T.);
#1394=FACE_OUTER_BOUND('',#2058,.T.);
#1395=FACE_OUTER_BOUND('',#2059,.T.);
#1396=FACE_OUTER_BOUND('',#2060,.T.);
#1397=FACE_OUTER_BOUND('',#2061,.T.);
#1398=FACE_OUTER_BOUND('',#2062,.T.);
#1399=FACE_OUTER_BOUND('',#2063,.T.);
#1400=FACE_OUTER_BOUND('',#2064,.T.);
#1401=FACE_OUTER_BOUND('',#2065,.T.);
#1402=FACE_OUTER_BOUND('',#2066,.T.);
#1403=FACE_OUTER_BOUND('',#2067,.T.);
#1404=FACE_OUTER_BOUND('',#2068,.T.);
#1405=FACE_OUTER_BOUND('',#2069,.T.);
#1406=FACE_OUTER_BOUND('',#2070,.T.);
#1407=FACE_OUTER_BOUND('',#2071,.T.);
#1408=FACE_OUTER_BOUND('',#2072,.T.);
#1409=FACE_OUTER_BOUND('',#2073,.T.);
#1410=FACE_OUTER_BOUND('',#2074,.T.);
#1411=FACE_OUTER_BOUND('',#2075,.T.);
#1412=FACE_OUTER_BOUND('',#2076,.T.);
#1413=FACE_OUTER_BOUND('',#2078,.T.);
#1414=FACE_OUTER_BOUND('',#2080,.T.);
#1415=FACE_OUTER_BOUND('',#2081,.T.);
#1416=FACE_OUTER_BOUND('',#2082,.T.);
#1417=FACE_OUTER_BOUND('',#2083,.T.);
#1418=FACE_OUTER_BOUND('',#2084,.T.);
#1419=FACE_OUTER_BOUND('',#2086,.T.);
#1420=FACE_OUTER_BOUND('',#2087,.T.);
#1421=FACE_OUTER_BOUND('',#2089,.T.);
#1422=FACE_OUTER_BOUND('',#2091,.T.);
#1423=FACE_OUTER_BOUND('',#2092,.T.);
#1424=FACE_OUTER_BOUND('',#2093,.T.);
#1425=FACE_OUTER_BOUND('',#2094,.T.);
#1426=FACE_OUTER_BOUND('',#2095,.T.);
#1427=FACE_OUTER_BOUND('',#2096,.T.);
#1428=FACE_OUTER_BOUND('',#2097,.T.);
#1429=FACE_OUTER_BOUND('',#2098,.T.);
#1430=FACE_OUTER_BOUND('',#2099,.T.);
#1431=FACE_OUTER_BOUND('',#2101,.T.);
#1432=FACE_OUTER_BOUND('',#2103,.T.);
#1433=FACE_OUTER_BOUND('',#2104,.T.);
#1434=FACE_OUTER_BOUND('',#2105,.T.);
#1435=FACE_OUTER_BOUND('',#2106,.T.);
#1436=FACE_OUTER_BOUND('',#2107,.T.);
#1437=FACE_OUTER_BOUND('',#2108,.T.);
#1438=FACE_OUTER_BOUND('',#2109,.T.);
#1439=FACE_OUTER_BOUND('',#2110,.T.);
#1440=FACE_OUTER_BOUND('',#2111,.T.);
#1441=FACE_OUTER_BOUND('',#2112,.T.);
#1442=FACE_OUTER_BOUND('',#2113,.T.);
#1443=FACE_OUTER_BOUND('',#2114,.T.);
#1444=FACE_OUTER_BOUND('',#2115,.T.);
#1445=FACE_OUTER_BOUND('',#2116,.T.);
#1446=FACE_OUTER_BOUND('',#2117,.T.);
#1447=FACE_OUTER_BOUND('',#2118,.T.);
#1448=FACE_OUTER_BOUND('',#2120,.T.);
#1449=FACE_OUTER_BOUND('',#2121,.T.);
#1450=FACE_OUTER_BOUND('',#2122,.T.);
#1451=FACE_OUTER_BOUND('',#2123,.T.);
#1452=FACE_OUTER_BOUND('',#2124,.T.);
#1453=FACE_OUTER_BOUND('',#2126,.T.);
#1454=FACE_OUTER_BOUND('',#2128,.T.);
#1455=FACE_OUTER_BOUND('',#2129,.T.);
#1456=FACE_OUTER_BOUND('',#2130,.T.);
#1457=FACE_OUTER_BOUND('',#2131,.T.);
#1458=FACE_OUTER_BOUND('',#2132,.T.);
#1459=FACE_OUTER_BOUND('',#2133,.T.);
#1460=FACE_OUTER_BOUND('',#2134,.T.);
#1461=FACE_OUTER_BOUND('',#2135,.T.);
#1462=EDGE_LOOP('',(#6597,#6598,#6599,#6600));
#1463=EDGE_LOOP('',(#6601,#6602,#6603,#6604));
#1464=EDGE_LOOP('',(#6605,#6606,#6607,#6608,#6609,#6610,#6611,#6612,#6613,
#6614,#6615,#6616,#6617,#6618,#6619,#6620,#6621,#6622,#6623,#6624,#6625,
#6626,#6627,#6628,#6629,#6630,#6631,#6632,#6633,#6634,#6635,#6636));
#1465=EDGE_LOOP('',(#6637,#6638,#6639,#6640));
#1466=EDGE_LOOP('',(#6641,#6642,#6643,#6644));
#1467=EDGE_LOOP('',(#6645,#6646,#6647,#6648));
#1468=EDGE_LOOP('',(#6649,#6650,#6651,#6652));
#1469=EDGE_LOOP('',(#6653,#6654,#6655,#6656));
#1470=EDGE_LOOP('',(#6657,#6658,#6659,#6660));
#1471=EDGE_LOOP('',(#6661,#6662,#6663,#6664));
#1472=EDGE_LOOP('',(#6665,#6666,#6667,#6668));
#1473=EDGE_LOOP('',(#6669,#6670,#6671,#6672));
#1474=EDGE_LOOP('',(#6673,#6674,#6675,#6676));
#1475=EDGE_LOOP('',(#6677,#6678,#6679,#6680,#6681,#6682,#6683,#6684,#6685,
#6686,#6687,#6688,#6689,#6690,#6691,#6692,#6693,#6694,#6695,#6696,#6697,
#6698,#6699,#6700,#6701,#6702,#6703,#6704));
#1476=EDGE_LOOP('',(#6705,#6706,#6707,#6708));
#1477=EDGE_LOOP('',(#6709,#6710,#6711,#6712,#6713,#6714));
#1478=EDGE_LOOP('',(#6715,#6716,#6717,#6718));
#1479=EDGE_LOOP('',(#6719,#6720,#6721,#6722));
#1480=EDGE_LOOP('',(#6723,#6724,#6725,#6726));
#1481=EDGE_LOOP('',(#6727,#6728,#6729,#6730));
#1482=EDGE_LOOP('',(#6731,#6732,#6733,#6734,#6735));
#1483=EDGE_LOOP('',(#6736,#6737,#6738,#6739,#6740));
#1484=EDGE_LOOP('',(#6741));
#1485=EDGE_LOOP('',(#6742,#6743,#6744,#6745));
#1486=EDGE_LOOP('',(#6746,#6747,#6748,#6749));
#1487=EDGE_LOOP('',(#6750,#6751,#6752,#6753));
#1488=EDGE_LOOP('',(#6754,#6755,#6756,#6757));
#1489=EDGE_LOOP('',(#6758,#6759,#6760,#6761,#6762));
#1490=EDGE_LOOP('',(#6763,#6764,#6765,#6766,#6767));
#1491=EDGE_LOOP('',(#6768));
#1492=EDGE_LOOP('',(#6769,#6770,#6771,#6772));
#1493=EDGE_LOOP('',(#6773,#6774,#6775,#6776));
#1494=EDGE_LOOP('',(#6777,#6778,#6779,#6780));
#1495=EDGE_LOOP('',(#6781,#6782,#6783,#6784));
#1496=EDGE_LOOP('',(#6785,#6786,#6787,#6788));
#1497=EDGE_LOOP('',(#6789,#6790,#6791,#6792));
#1498=EDGE_LOOP('',(#6793,#6794,#6795,#6796));
#1499=EDGE_LOOP('',(#6797,#6798,#6799,#6800));
#1500=EDGE_LOOP('',(#6801,#6802,#6803,#6804));
#1501=EDGE_LOOP('',(#6805,#6806,#6807,#6808));
#1502=EDGE_LOOP('',(#6809,#6810,#6811,#6812));
#1503=EDGE_LOOP('',(#6813,#6814,#6815,#6816));
#1504=EDGE_LOOP('',(#6817,#6818,#6819,#6820));
#1505=EDGE_LOOP('',(#6821,#6822,#6823,#6824));
#1506=EDGE_LOOP('',(#6825,#6826,#6827,#6828));
#1507=EDGE_LOOP('',(#6829,#6830,#6831,#6832));
#1508=EDGE_LOOP('',(#6833,#6834,#6835,#6836));
#1509=EDGE_LOOP('',(#6837,#6838,#6839,#6840));
#1510=EDGE_LOOP('',(#6841));
#1511=EDGE_LOOP('',(#6842));
#1512=EDGE_LOOP('',(#6843,#6844));
#1513=EDGE_LOOP('',(#6845,#6846,#6847,#6848));
#1514=EDGE_LOOP('',(#6849,#6850,#6851,#6852));
#1515=EDGE_LOOP('',(#6853,#6854,#6855,#6856));
#1516=EDGE_LOOP('',(#6857,#6858,#6859,#6860));
#1517=EDGE_LOOP('',(#6861,#6862,#6863,#6864,#6865,#6866));
#1518=EDGE_LOOP('',(#6867,#6868,#6869,#6870,#6871,#6872));
#1519=EDGE_LOOP('',(#6873,#6874,#6875,#6876,#6877,#6878));
#1520=EDGE_LOOP('',(#6879,#6880,#6881,#6882,#6883,#6884,#6885,#6886));
#1521=EDGE_LOOP('',(#6887,#6888,#6889,#6890));
#1522=EDGE_LOOP('',(#6891,#6892,#6893,#6894));
#1523=EDGE_LOOP('',(#6895,#6896,#6897,#6898));
#1524=EDGE_LOOP('',(#6899,#6900,#6901));
#1525=EDGE_LOOP('',(#6902,#6903,#6904));
#1526=EDGE_LOOP('',(#6905,#6906,#6907));
#1527=EDGE_LOOP('',(#6908,#6909,#6910,#6911));
#1528=EDGE_LOOP('',(#6912,#6913,#6914,#6915));
#1529=EDGE_LOOP('',(#6916,#6917,#6918,#6919));
#1530=EDGE_LOOP('',(#6920,#6921,#6922,#6923));
#1531=EDGE_LOOP('',(#6924,#6925,#6926,#6927));
#1532=EDGE_LOOP('',(#6928,#6929,#6930,#6931));
#1533=EDGE_LOOP('',(#6932,#6933,#6934,#6935));
#1534=EDGE_LOOP('',(#6936,#6937,#6938,#6939));
#1535=EDGE_LOOP('',(#6940));
#1536=EDGE_LOOP('',(#6941));
#1537=EDGE_LOOP('',(#6942));
#1538=EDGE_LOOP('',(#6943,#6944,#6945,#6946));
#1539=EDGE_LOOP('',(#6947,#6948,#6949,#6950,#6951,#6952));
#1540=EDGE_LOOP('',(#6953,#6954,#6955,#6956,#6957,#6958,#6959,#6960,#6961,
#6962,#6963,#6964));
#1541=EDGE_LOOP('',(#6965,#6966,#6967,#6968,#6969,#6970,#6971,#6972,#6973,
#6974,#6975,#6976));
#1542=EDGE_LOOP('',(#6977,#6978,#6979,#6980));
#1543=EDGE_LOOP('',(#6981,#6982,#6983,#6984));
#1544=EDGE_LOOP('',(#6985,#6986,#6987,#6988));
#1545=EDGE_LOOP('',(#6989,#6990,#6991,#6992));
#1546=EDGE_LOOP('',(#6993,#6994,#6995,#6996,#6997));
#1547=EDGE_LOOP('',(#6998));
#1548=EDGE_LOOP('',(#6999,#7000,#7001,#7002,#7003));
#1549=EDGE_LOOP('',(#7004,#7005,#7006,#7007));
#1550=EDGE_LOOP('',(#7008,#7009,#7010,#7011));
#1551=EDGE_LOOP('',(#7012,#7013,#7014,#7015));
#1552=EDGE_LOOP('',(#7016,#7017,#7018,#7019));
#1553=EDGE_LOOP('',(#7020,#7021,#7022,#7023,#7024));
#1554=EDGE_LOOP('',(#7025));
#1555=EDGE_LOOP('',(#7026,#7027,#7028,#7029,#7030));
#1556=EDGE_LOOP('',(#7031,#7032));
#1557=EDGE_LOOP('',(#7033,#7034));
#1558=EDGE_LOOP('',(#7035,#7036));
#1559=EDGE_LOOP('',(#7037));
#1560=EDGE_LOOP('',(#7038));
#1561=EDGE_LOOP('',(#7039,#7040));
#1562=EDGE_LOOP('',(#7041,#7042,#7043,#7044,#7045,#7046));
#1563=EDGE_LOOP('',(#7047,#7048,#7049,#7050,#7051,#7052));
#1564=EDGE_LOOP('',(#7053,#7054,#7055,#7056,#7057,#7058));
#1565=EDGE_LOOP('',(#7059,#7060,#7061,#7062));
#1566=EDGE_LOOP('',(#7063,#7064,#7065,#7066));
#1567=EDGE_LOOP('',(#7067,#7068,#7069,#7070));
#1568=EDGE_LOOP('',(#7071,#7072,#7073,#7074,#7075,#7076,#7077,#7078,#7079,
#7080,#7081,#7082));
#1569=EDGE_LOOP('',(#7083,#7084,#7085,#7086,#7087,#7088,#7089,#7090,#7091,
#7092,#7093,#7094));
#1570=EDGE_LOOP('',(#7095,#7096,#7097,#7098,#7099,#7100,#7101,#7102,#7103,
#7104,#7105,#7106));
#1571=EDGE_LOOP('',(#7107,#7108,#7109,#7110,#7111,#7112,#7113,#7114));
#1572=EDGE_LOOP('',(#7115,#7116,#7117,#7118));
#1573=EDGE_LOOP('',(#7119,#7120,#7121,#7122));
#1574=EDGE_LOOP('',(#7123,#7124,#7125,#7126));
#1575=EDGE_LOOP('',(#7127,#7128,#7129,#7130));
#1576=EDGE_LOOP('',(#7131,#7132,#7133,#7134));
#1577=EDGE_LOOP('',(#7135,#7136,#7137,#7138));
#1578=EDGE_LOOP('',(#7139,#7140,#7141,#7142));
#1579=EDGE_LOOP('',(#7143,#7144,#7145,#7146));
#1580=EDGE_LOOP('',(#7147,#7148,#7149,#7150));
#1581=EDGE_LOOP('',(#7151,#7152,#7153,#7154));
#1582=EDGE_LOOP('',(#7155,#7156,#7157,#7158));
#1583=EDGE_LOOP('',(#7159,#7160));
#1584=EDGE_LOOP('',(#7161,#7162));
#1585=EDGE_LOOP('',(#7163,#7164));
#1586=EDGE_LOOP('',(#7165,#7166,#7167,#7168,#7169,#7170,#7171,#7172));
#1587=EDGE_LOOP('',(#7173));
#1588=EDGE_LOOP('',(#7174));
#1589=EDGE_LOOP('',(#7175));
#1590=EDGE_LOOP('',(#7176,#7177,#7178,#7179));
#1591=EDGE_LOOP('',(#7180,#7181,#7182,#7183));
#1592=EDGE_LOOP('',(#7184,#7185,#7186,#7187));
#1593=EDGE_LOOP('',(#7188,#7189,#7190,#7191));
#1594=EDGE_LOOP('',(#7192,#7193,#7194,#7195,#7196,#7197,#7198,#7199));
#1595=EDGE_LOOP('',(#7200,#7201,#7202,#7203,#7204,#7205,#7206,#7207));
#1596=EDGE_LOOP('',(#7208,#7209,#7210,#7211,#7212,#7213,#7214,#7215,#7216,
#7217));
#1597=EDGE_LOOP('',(#7218));
#1598=EDGE_LOOP('',(#7219,#7220,#7221,#7222));
#1599=EDGE_LOOP('',(#7223,#7224,#7225,#7226,#7227,#7228,#7229,#7230,#7231,
#7232));
#1600=EDGE_LOOP('',(#7233,#7234,#7235,#7236));
#1601=EDGE_LOOP('',(#7237,#7238,#7239,#7240));
#1602=EDGE_LOOP('',(#7241,#7242,#7243,#7244));
#1603=EDGE_LOOP('',(#7245,#7246,#7247,#7248));
#1604=EDGE_LOOP('',(#7249,#7250,#7251,#7252));
#1605=EDGE_LOOP('',(#7253,#7254,#7255,#7256,#7257,#7258));
#1606=EDGE_LOOP('',(#7259));
#1607=EDGE_LOOP('',(#7260));
#1608=EDGE_LOOP('',(#7261,#7262,#7263,#7264));
#1609=EDGE_LOOP('',(#7265,#7266,#7267,#7268));
#1610=EDGE_LOOP('',(#7269,#7270,#7271,#7272));
#1611=EDGE_LOOP('',(#7273,#7274,#7275,#7276));
#1612=EDGE_LOOP('',(#7277,#7278,#7279,#7280));
#1613=EDGE_LOOP('',(#7281,#7282,#7283,#7284,#7285,#7286));
#1614=EDGE_LOOP('',(#7287));
#1615=EDGE_LOOP('',(#7288,#7289,#7290,#7291,#7292,#7293,#7294,#7295));
#1616=EDGE_LOOP('',(#7296,#7297,#7298,#7299,#7300,#7301,#7302,#7303));
#1617=EDGE_LOOP('',(#7304,#7305,#7306,#7307,#7308,#7309,#7310,#7311,#7312,
#7313,#7314,#7315,#7316,#7317));
#1618=EDGE_LOOP('',(#7318,#7319,#7320,#7321,#7322,#7323,#7324,#7325,#7326,
#7327,#7328,#7329,#7330,#7331));
#1619=EDGE_LOOP('',(#7332));
#1620=EDGE_LOOP('',(#7333));
#1621=EDGE_LOOP('',(#7334,#7335,#7336));
#1622=EDGE_LOOP('',(#7337,#7338,#7339));
#1623=EDGE_LOOP('',(#7340,#7341,#7342));
#1624=EDGE_LOOP('',(#7343,#7344,#7345,#7346));
#1625=EDGE_LOOP('',(#7347,#7348,#7349,#7350));
#1626=EDGE_LOOP('',(#7351,#7352,#7353,#7354));
#1627=EDGE_LOOP('',(#7355,#7356,#7357,#7358));
#1628=EDGE_LOOP('',(#7359,#7360,#7361,#7362));
#1629=EDGE_LOOP('',(#7363,#7364,#7365,#7366));
#1630=EDGE_LOOP('',(#7367,#7368,#7369,#7370));
#1631=EDGE_LOOP('',(#7371,#7372,#7373,#7374));
#1632=EDGE_LOOP('',(#7375,#7376,#7377,#7378));
#1633=EDGE_LOOP('',(#7379,#7380,#7381,#7382));
#1634=EDGE_LOOP('',(#7383,#7384,#7385,#7386));
#1635=EDGE_LOOP('',(#7387,#7388,#7389,#7390));
#1636=EDGE_LOOP('',(#7391,#7392,#7393,#7394));
#1637=EDGE_LOOP('',(#7395,#7396,#7397,#7398));
#1638=EDGE_LOOP('',(#7399,#7400,#7401,#7402));
#1639=EDGE_LOOP('',(#7403,#7404,#7405,#7406));
#1640=EDGE_LOOP('',(#7407,#7408,#7409,#7410));
#1641=EDGE_LOOP('',(#7411,#7412,#7413,#7414));
#1642=EDGE_LOOP('',(#7415,#7416,#7417,#7418));
#1643=EDGE_LOOP('',(#7419,#7420,#7421,#7422,#7423,#7424,#7425,#7426,#7427,
#7428));
#1644=EDGE_LOOP('',(#7429));
#1645=EDGE_LOOP('',(#7430));
#1646=EDGE_LOOP('',(#7431,#7432,#7433,#7434,#7435,#7436,#7437,#7438,#7439,
#7440));
#1647=EDGE_LOOP('',(#7441));
#1648=EDGE_LOOP('',(#7442,#7443,#7444,#7445));
#1649=EDGE_LOOP('',(#7446,#7447,#7448,#7449));
#1650=EDGE_LOOP('',(#7450,#7451,#7452,#7453));
#1651=EDGE_LOOP('',(#7454));
#1652=EDGE_LOOP('',(#7455));
#1653=EDGE_LOOP('',(#7456));
#1654=EDGE_LOOP('',(#7457));
#1655=EDGE_LOOP('',(#7458));
#1656=EDGE_LOOP('',(#7459));
#1657=EDGE_LOOP('',(#7460));
#1658=EDGE_LOOP('',(#7461,#7462,#7463,#7464));
#1659=EDGE_LOOP('',(#7465,#7466,#7467,#7468));
#1660=EDGE_LOOP('',(#7469,#7470,#7471,#7472));
#1661=EDGE_LOOP('',(#7473,#7474,#7475,#7476));
#1662=EDGE_LOOP('',(#7477,#7478,#7479,#7480));
#1663=EDGE_LOOP('',(#7481,#7482,#7483,#7484));
#1664=EDGE_LOOP('',(#7485,#7486,#7487,#7488));
#1665=EDGE_LOOP('',(#7489,#7490,#7491,#7492));
#1666=EDGE_LOOP('',(#7493,#7494,#7495,#7496));
#1667=EDGE_LOOP('',(#7497,#7498,#7499,#7500));
#1668=EDGE_LOOP('',(#7501,#7502,#7503,#7504));
#1669=EDGE_LOOP('',(#7505,#7506,#7507,#7508));
#1670=EDGE_LOOP('',(#7509,#7510,#7511,#7512));
#1671=EDGE_LOOP('',(#7513,#7514,#7515,#7516));
#1672=EDGE_LOOP('',(#7517,#7518,#7519,#7520));
#1673=EDGE_LOOP('',(#7521,#7522,#7523,#7524));
#1674=EDGE_LOOP('',(#7525,#7526,#7527,#7528));
#1675=EDGE_LOOP('',(#7529,#7530,#7531,#7532));
#1676=EDGE_LOOP('',(#7533,#7534,#7535,#7536));
#1677=EDGE_LOOP('',(#7537,#7538,#7539,#7540));
#1678=EDGE_LOOP('',(#7541,#7542,#7543,#7544));
#1679=EDGE_LOOP('',(#7545));
#1680=EDGE_LOOP('',(#7546));
#1681=EDGE_LOOP('',(#7547,#7548,#7549,#7550));
#1682=EDGE_LOOP('',(#7551));
#1683=EDGE_LOOP('',(#7552));
#1684=EDGE_LOOP('',(#7553));
#1685=EDGE_LOOP('',(#7554));
#1686=EDGE_LOOP('',(#7555));
#1687=EDGE_LOOP('',(#7556));
#1688=EDGE_LOOP('',(#7557,#7558,#7559,#7560));
#1689=EDGE_LOOP('',(#7561,#7562,#7563,#7564));
#1690=EDGE_LOOP('',(#7565,#7566,#7567,#7568));
#1691=EDGE_LOOP('',(#7569,#7570,#7571,#7572));
#1692=EDGE_LOOP('',(#7573,#7574,#7575,#7576));
#1693=EDGE_LOOP('',(#7577));
#1694=EDGE_LOOP('',(#7578));
#1695=EDGE_LOOP('',(#7579));
#1696=EDGE_LOOP('',(#7580));
#1697=EDGE_LOOP('',(#7581));
#1698=EDGE_LOOP('',(#7582));
#1699=EDGE_LOOP('',(#7583));
#1700=EDGE_LOOP('',(#7584));
#1701=EDGE_LOOP('',(#7585));
#1702=EDGE_LOOP('',(#7586));
#1703=EDGE_LOOP('',(#7587,#7588,#7589,#7590));
#1704=EDGE_LOOP('',(#7591,#7592,#7593,#7594));
#1705=EDGE_LOOP('',(#7595,#7596,#7597,#7598));
#1706=EDGE_LOOP('',(#7599,#7600,#7601,#7602));
#1707=EDGE_LOOP('',(#7603,#7604,#7605,#7606));
#1708=EDGE_LOOP('',(#7607));
#1709=EDGE_LOOP('',(#7608));
#1710=EDGE_LOOP('',(#7609));
#1711=EDGE_LOOP('',(#7610));
#1712=EDGE_LOOP('',(#7611));
#1713=EDGE_LOOP('',(#7612));
#1714=EDGE_LOOP('',(#7613));
#1715=EDGE_LOOP('',(#7614));
#1716=EDGE_LOOP('',(#7615));
#1717=EDGE_LOOP('',(#7616));
#1718=EDGE_LOOP('',(#7617,#7618,#7619,#7620,#7621));
#1719=EDGE_LOOP('',(#7622,#7623,#7624,#7625,#7626));
#1720=EDGE_LOOP('',(#7627,#7628,#7629,#7630));
#1721=EDGE_LOOP('',(#7631,#7632,#7633,#7634));
#1722=EDGE_LOOP('',(#7635,#7636,#7637,#7638,#7639,#7640,#7641,#7642,#7643,
#7644,#7645,#7646,#7647,#7648,#7649,#7650));
#1723=EDGE_LOOP('',(#7651,#7652));
#1724=EDGE_LOOP('',(#7653,#7654));
#1725=EDGE_LOOP('',(#7655,#7656,#7657));
#1726=EDGE_LOOP('',(#7658));
#1727=EDGE_LOOP('',(#7659));
#1728=EDGE_LOOP('',(#7660));
#1729=EDGE_LOOP('',(#7661));
#1730=EDGE_LOOP('',(#7662));
#1731=EDGE_LOOP('',(#7663,#7664,#7665,#7666));
#1732=EDGE_LOOP('',(#7667));
#1733=EDGE_LOOP('',(#7668,#7669,#7670,#7671));
#1734=EDGE_LOOP('',(#7672));
#1735=EDGE_LOOP('',(#7673,#7674,#7675,#7676));
#1736=EDGE_LOOP('',(#7677,#7678,#7679,#7680));
#1737=EDGE_LOOP('',(#7681,#7682,#7683,#7684));
#1738=EDGE_LOOP('',(#7685));
#1739=EDGE_LOOP('',(#7686,#7687,#7688,#7689));
#1740=EDGE_LOOP('',(#7690));
#1741=EDGE_LOOP('',(#7691,#7692,#7693,#7694));
#1742=EDGE_LOOP('',(#7695,#7696,#7697,#7698));
#1743=EDGE_LOOP('',(#7699,#7700,#7701,#7702));
#1744=EDGE_LOOP('',(#7703,#7704,#7705,#7706));
#1745=EDGE_LOOP('',(#7707,#7708,#7709,#7710));
#1746=EDGE_LOOP('',(#7711,#7712,#7713,#7714));
#1747=EDGE_LOOP('',(#7715));
#1748=EDGE_LOOP('',(#7716,#7717,#7718,#7719));
#1749=EDGE_LOOP('',(#7720));
#1750=EDGE_LOOP('',(#7721,#7722,#7723,#7724));
#1751=EDGE_LOOP('',(#7725,#7726,#7727,#7728));
#1752=EDGE_LOOP('',(#7729,#7730,#7731,#7732));
#1753=EDGE_LOOP('',(#7733,#7734,#7735,#7736));
#1754=EDGE_LOOP('',(#7737,#7738,#7739,#7740));
#1755=EDGE_LOOP('',(#7741,#7742,#7743,#7744));
#1756=EDGE_LOOP('',(#7745,#7746,#7747,#7748));
#1757=EDGE_LOOP('',(#7749,#7750,#7751,#7752,#7753));
#1758=EDGE_LOOP('',(#7754));
#1759=EDGE_LOOP('',(#7755));
#1760=EDGE_LOOP('',(#7756));
#1761=EDGE_LOOP('',(#7757));
#1762=EDGE_LOOP('',(#7758));
#1763=EDGE_LOOP('',(#7759));
#1764=EDGE_LOOP('',(#7760));
#1765=EDGE_LOOP('',(#7761,#7762,#7763,#7764));
#1766=EDGE_LOOP('',(#7765));
#1767=EDGE_LOOP('',(#7766));
#1768=EDGE_LOOP('',(#7767,#7768,#7769,#7770));
#1769=EDGE_LOOP('',(#7771,#7772,#7773,#7774));
#1770=EDGE_LOOP('',(#7775,#7776,#7777,#7778));
#1771=EDGE_LOOP('',(#7779,#7780,#7781,#7782));
#1772=EDGE_LOOP('',(#7783,#7784,#7785,#7786));
#1773=EDGE_LOOP('',(#7787,#7788,#7789,#7790));
#1774=EDGE_LOOP('',(#7791,#7792,#7793,#7794));
#1775=EDGE_LOOP('',(#7795,#7796,#7797,#7798));
#1776=EDGE_LOOP('',(#7799,#7800,#7801,#7802));
#1777=EDGE_LOOP('',(#7803));
#1778=EDGE_LOOP('',(#7804));
#1779=EDGE_LOOP('',(#7805,#7806,#7807,#7808));
#1780=EDGE_LOOP('',(#7809));
#1781=EDGE_LOOP('',(#7810));
#1782=EDGE_LOOP('',(#7811));
#1783=EDGE_LOOP('',(#7812));
#1784=EDGE_LOOP('',(#7813));
#1785=EDGE_LOOP('',(#7814));
#1786=EDGE_LOOP('',(#7815,#7816,#7817,#7818));
#1787=EDGE_LOOP('',(#7819,#7820,#7821,#7822));
#1788=EDGE_LOOP('',(#7823,#7824,#7825,#7826));
#1789=EDGE_LOOP('',(#7827,#7828,#7829,#7830,#7831,#7832,#7833,#7834));
#1790=EDGE_LOOP('',(#7835));
#1791=EDGE_LOOP('',(#7836));
#1792=EDGE_LOOP('',(#7837));
#1793=EDGE_LOOP('',(#7838,#7839,#7840,#7841,#7842,#7843,#7844,#7845));
#1794=EDGE_LOOP('',(#7846));
#1795=EDGE_LOOP('',(#7847));
#1796=EDGE_LOOP('',(#7848));
#1797=EDGE_LOOP('',(#7849,#7850,#7851,#7852));
#1798=EDGE_LOOP('',(#7853,#7854,#7855,#7856));
#1799=EDGE_LOOP('',(#7857,#7858,#7859,#7860));
#1800=EDGE_LOOP('',(#7861,#7862,#7863,#7864));
#1801=EDGE_LOOP('',(#7865,#7866,#7867,#7868));
#1802=EDGE_LOOP('',(#7869,#7870,#7871,#7872));
#1803=EDGE_LOOP('',(#7873,#7874,#7875,#7876));
#1804=EDGE_LOOP('',(#7877,#7878,#7879,#7880));
#1805=EDGE_LOOP('',(#7881,#7882,#7883,#7884));
#1806=EDGE_LOOP('',(#7885,#7886,#7887,#7888,#7889,#7890,#7891,#7892,#7893,
#7894,#7895,#7896));
#1807=EDGE_LOOP('',(#7897,#7898,#7899,#7900));
#1808=EDGE_LOOP('',(#7901,#7902,#7903,#7904));
#1809=EDGE_LOOP('',(#7905,#7906,#7907,#7908));
#1810=EDGE_LOOP('',(#7909,#7910,#7911,#7912));
#1811=EDGE_LOOP('',(#7913,#7914,#7915,#7916));
#1812=EDGE_LOOP('',(#7917,#7918,#7919,#7920));
#1813=EDGE_LOOP('',(#7921,#7922,#7923,#7924));
#1814=EDGE_LOOP('',(#7925,#7926,#7927,#7928));
#1815=EDGE_LOOP('',(#7929,#7930,#7931,#7932));
#1816=EDGE_LOOP('',(#7933,#7934,#7935,#7936));
#1817=EDGE_LOOP('',(#7937,#7938,#7939,#7940));
#1818=EDGE_LOOP('',(#7941,#7942,#7943,#7944));
#1819=EDGE_LOOP('',(#7945,#7946,#7947,#7948));
#1820=EDGE_LOOP('',(#7949,#7950,#7951,#7952));
#1821=EDGE_LOOP('',(#7953,#7954,#7955,#7956));
#1822=EDGE_LOOP('',(#7957,#7958,#7959,#7960));
#1823=EDGE_LOOP('',(#7961,#7962,#7963,#7964));
#1824=EDGE_LOOP('',(#7965,#7966,#7967,#7968));
#1825=EDGE_LOOP('',(#7969,#7970,#7971,#7972));
#1826=EDGE_LOOP('',(#7973,#7974,#7975,#7976));
#1827=EDGE_LOOP('',(#7977,#7978,#7979,#7980));
#1828=EDGE_LOOP('',(#7981,#7982,#7983,#7984));
#1829=EDGE_LOOP('',(#7985,#7986,#7987,#7988));
#1830=EDGE_LOOP('',(#7989,#7990,#7991,#7992));
#1831=EDGE_LOOP('',(#7993,#7994,#7995,#7996));
#1832=EDGE_LOOP('',(#7997,#7998,#7999,#8000));
#1833=EDGE_LOOP('',(#8001,#8002,#8003,#8004));
#1834=EDGE_LOOP('',(#8005,#8006,#8007,#8008));
#1835=EDGE_LOOP('',(#8009,#8010,#8011,#8012));
#1836=EDGE_LOOP('',(#8013,#8014,#8015,#8016));
#1837=EDGE_LOOP('',(#8017,#8018,#8019,#8020));
#1838=EDGE_LOOP('',(#8021,#8022,#8023,#8024));
#1839=EDGE_LOOP('',(#8025,#8026,#8027,#8028));
#1840=EDGE_LOOP('',(#8029,#8030,#8031,#8032));
#1841=EDGE_LOOP('',(#8033,#8034,#8035,#8036));
#1842=EDGE_LOOP('',(#8037,#8038,#8039,#8040));
#1843=EDGE_LOOP('',(#8041,#8042,#8043,#8044));
#1844=EDGE_LOOP('',(#8045,#8046,#8047,#8048));
#1845=EDGE_LOOP('',(#8049,#8050,#8051,#8052));
#1846=EDGE_LOOP('',(#8053));
#1847=EDGE_LOOP('',(#8054));
#1848=EDGE_LOOP('',(#8055));
#1849=EDGE_LOOP('',(#8056));
#1850=EDGE_LOOP('',(#8057,#8058,#8059,#8060));
#1851=EDGE_LOOP('',(#8061,#8062,#8063,#8064));
#1852=EDGE_LOOP('',(#8065,#8066,#8067,#8068));
#1853=EDGE_LOOP('',(#8069,#8070,#8071,#8072));
#1854=EDGE_LOOP('',(#8073,#8074,#8075,#8076));
#1855=EDGE_LOOP('',(#8077,#8078,#8079,#8080));
#1856=EDGE_LOOP('',(#8081,#8082,#8083,#8084));
#1857=EDGE_LOOP('',(#8085,#8086,#8087,#8088));
#1858=EDGE_LOOP('',(#8089,#8090,#8091,#8092));
#1859=EDGE_LOOP('',(#8093,#8094,#8095,#8096));
#1860=EDGE_LOOP('',(#8097,#8098,#8099,#8100));
#1861=EDGE_LOOP('',(#8101,#8102,#8103,#8104));
#1862=EDGE_LOOP('',(#8105,#8106,#8107,#8108));
#1863=EDGE_LOOP('',(#8109,#8110,#8111,#8112));
#1864=EDGE_LOOP('',(#8113,#8114,#8115,#8116));
#1865=EDGE_LOOP('',(#8117,#8118,#8119,#8120));
#1866=EDGE_LOOP('',(#8121,#8122,#8123,#8124));
#1867=EDGE_LOOP('',(#8125,#8126,#8127,#8128));
#1868=EDGE_LOOP('',(#8129,#8130,#8131,#8132));
#1869=EDGE_LOOP('',(#8133,#8134,#8135,#8136));
#1870=EDGE_LOOP('',(#8137,#8138,#8139,#8140));
#1871=EDGE_LOOP('',(#8141,#8142,#8143,#8144));
#1872=EDGE_LOOP('',(#8145,#8146,#8147,#8148));
#1873=EDGE_LOOP('',(#8149,#8150,#8151,#8152));
#1874=EDGE_LOOP('',(#8153,#8154,#8155,#8156));
#1875=EDGE_LOOP('',(#8157,#8158,#8159,#8160));
#1876=EDGE_LOOP('',(#8161,#8162,#8163,#8164));
#1877=EDGE_LOOP('',(#8165,#8166,#8167,#8168));
#1878=EDGE_LOOP('',(#8169,#8170,#8171,#8172));
#1879=EDGE_LOOP('',(#8173,#8174,#8175,#8176));
#1880=EDGE_LOOP('',(#8177,#8178,#8179,#8180));
#1881=EDGE_LOOP('',(#8181,#8182,#8183,#8184));
#1882=EDGE_LOOP('',(#8185,#8186,#8187,#8188));
#1883=EDGE_LOOP('',(#8189,#8190,#8191,#8192));
#1884=EDGE_LOOP('',(#8193,#8194,#8195,#8196));
#1885=EDGE_LOOP('',(#8197,#8198,#8199,#8200));
#1886=EDGE_LOOP('',(#8201,#8202,#8203,#8204));
#1887=EDGE_LOOP('',(#8205,#8206,#8207,#8208,#8209));
#1888=EDGE_LOOP('',(#8210,#8211,#8212,#8213,#8214));
#1889=EDGE_LOOP('',(#8215,#8216,#8217,#8218));
#1890=EDGE_LOOP('',(#8219,#8220,#8221,#8222));
#1891=EDGE_LOOP('',(#8223,#8224,#8225,#8226));
#1892=EDGE_LOOP('',(#8227,#8228,#8229,#8230));
#1893=EDGE_LOOP('',(#8231,#8232,#8233,#8234));
#1894=EDGE_LOOP('',(#8235,#8236,#8237,#8238));
#1895=EDGE_LOOP('',(#8239,#8240,#8241,#8242));
#1896=EDGE_LOOP('',(#8243,#8244,#8245,#8246));
#1897=EDGE_LOOP('',(#8247,#8248,#8249,#8250));
#1898=EDGE_LOOP('',(#8251,#8252,#8253,#8254));
#1899=EDGE_LOOP('',(#8255,#8256,#8257,#8258));
#1900=EDGE_LOOP('',(#8259,#8260,#8261,#8262));
#1901=EDGE_LOOP('',(#8263,#8264,#8265,#8266));
#1902=EDGE_LOOP('',(#8267,#8268,#8269,#8270));
#1903=EDGE_LOOP('',(#8271,#8272,#8273,#8274));
#1904=EDGE_LOOP('',(#8275,#8276,#8277,#8278));
#1905=EDGE_LOOP('',(#8279,#8280,#8281,#8282));
#1906=EDGE_LOOP('',(#8283,#8284,#8285,#8286));
#1907=EDGE_LOOP('',(#8287,#8288,#8289,#8290));
#1908=EDGE_LOOP('',(#8291,#8292,#8293,#8294));
#1909=EDGE_LOOP('',(#8295,#8296,#8297,#8298));
#1910=EDGE_LOOP('',(#8299,#8300,#8301,#8302));
#1911=EDGE_LOOP('',(#8303,#8304,#8305,#8306));
#1912=EDGE_LOOP('',(#8307,#8308,#8309,#8310));
#1913=EDGE_LOOP('',(#8311,#8312,#8313,#8314));
#1914=EDGE_LOOP('',(#8315,#8316,#8317,#8318));
#1915=EDGE_LOOP('',(#8319,#8320,#8321,#8322));
#1916=EDGE_LOOP('',(#8323,#8324,#8325,#8326));
#1917=EDGE_LOOP('',(#8327,#8328,#8329,#8330));
#1918=EDGE_LOOP('',(#8331,#8332,#8333,#8334));
#1919=EDGE_LOOP('',(#8335,#8336,#8337,#8338));
#1920=EDGE_LOOP('',(#8339,#8340,#8341,#8342));
#1921=EDGE_LOOP('',(#8343,#8344,#8345,#8346));
#1922=EDGE_LOOP('',(#8347,#8348,#8349,#8350));
#1923=EDGE_LOOP('',(#8351,#8352,#8353,#8354));
#1924=EDGE_LOOP('',(#8355,#8356,#8357,#8358));
#1925=EDGE_LOOP('',(#8359,#8360,#8361,#8362));
#1926=EDGE_LOOP('',(#8363,#8364,#8365,#8366));
#1927=EDGE_LOOP('',(#8367,#8368,#8369,#8370));
#1928=EDGE_LOOP('',(#8371,#8372,#8373,#8374));
#1929=EDGE_LOOP('',(#8375,#8376,#8377,#8378));
#1930=EDGE_LOOP('',(#8379,#8380,#8381,#8382));
#1931=EDGE_LOOP('',(#8383,#8384,#8385,#8386));
#1932=EDGE_LOOP('',(#8387,#8388,#8389,#8390));
#1933=EDGE_LOOP('',(#8391,#8392,#8393,#8394));
#1934=EDGE_LOOP('',(#8395,#8396,#8397,#8398));
#1935=EDGE_LOOP('',(#8399,#8400,#8401,#8402));
#1936=EDGE_LOOP('',(#8403,#8404,#8405,#8406));
#1937=EDGE_LOOP('',(#8407,#8408,#8409,#8410));
#1938=EDGE_LOOP('',(#8411,#8412,#8413,#8414));
#1939=EDGE_LOOP('',(#8415,#8416,#8417,#8418));
#1940=EDGE_LOOP('',(#8419,#8420,#8421,#8422));
#1941=EDGE_LOOP('',(#8423,#8424,#8425,#8426));
#1942=EDGE_LOOP('',(#8427,#8428,#8429,#8430));
#1943=EDGE_LOOP('',(#8431,#8432,#8433,#8434));
#1944=EDGE_LOOP('',(#8435,#8436,#8437,#8438));
#1945=EDGE_LOOP('',(#8439,#8440,#8441,#8442));
#1946=EDGE_LOOP('',(#8443,#8444,#8445,#8446));
#1947=EDGE_LOOP('',(#8447,#8448,#8449,#8450));
#1948=EDGE_LOOP('',(#8451,#8452,#8453,#8454));
#1949=EDGE_LOOP('',(#8455,#8456,#8457,#8458));
#1950=EDGE_LOOP('',(#8459,#8460,#8461,#8462));
#1951=EDGE_LOOP('',(#8463,#8464,#8465,#8466));
#1952=EDGE_LOOP('',(#8467,#8468,#8469,#8470));
#1953=EDGE_LOOP('',(#8471,#8472,#8473,#8474));
#1954=EDGE_LOOP('',(#8475,#8476,#8477,#8478));
#1955=EDGE_LOOP('',(#8479,#8480,#8481,#8482));
#1956=EDGE_LOOP('',(#8483,#8484,#8485,#8486));
#1957=EDGE_LOOP('',(#8487,#8488,#8489,#8490));
#1958=EDGE_LOOP('',(#8491,#8492,#8493,#8494));
#1959=EDGE_LOOP('',(#8495,#8496,#8497,#8498));
#1960=EDGE_LOOP('',(#8499,#8500,#8501,#8502));
#1961=EDGE_LOOP('',(#8503,#8504,#8505,#8506));
#1962=EDGE_LOOP('',(#8507,#8508,#8509,#8510));
#1963=EDGE_LOOP('',(#8511,#8512,#8513,#8514));
#1964=EDGE_LOOP('',(#8515,#8516,#8517,#8518));
#1965=EDGE_LOOP('',(#8519,#8520,#8521,#8522));
#1966=EDGE_LOOP('',(#8523,#8524,#8525,#8526));
#1967=EDGE_LOOP('',(#8527,#8528,#8529,#8530));
#1968=EDGE_LOOP('',(#8531,#8532,#8533,#8534));
#1969=EDGE_LOOP('',(#8535,#8536,#8537,#8538));
#1970=EDGE_LOOP('',(#8539,#8540,#8541,#8542));
#1971=EDGE_LOOP('',(#8543,#8544,#8545,#8546));
#1972=EDGE_LOOP('',(#8547,#8548,#8549,#8550));
#1973=EDGE_LOOP('',(#8551,#8552,#8553,#8554));
#1974=EDGE_LOOP('',(#8555,#8556,#8557,#8558));
#1975=EDGE_LOOP('',(#8559,#8560,#8561,#8562));
#1976=EDGE_LOOP('',(#8563,#8564,#8565,#8566));
#1977=EDGE_LOOP('',(#8567,#8568,#8569,#8570));
#1978=EDGE_LOOP('',(#8571,#8572,#8573,#8574));
#1979=EDGE_LOOP('',(#8575,#8576,#8577,#8578));
#1980=EDGE_LOOP('',(#8579,#8580,#8581,#8582));
#1981=EDGE_LOOP('',(#8583,#8584,#8585,#8586));
#1982=EDGE_LOOP('',(#8587,#8588,#8589,#8590));
#1983=EDGE_LOOP('',(#8591,#8592,#8593,#8594));
#1984=EDGE_LOOP('',(#8595,#8596,#8597,#8598));
#1985=EDGE_LOOP('',(#8599,#8600,#8601,#8602));
#1986=EDGE_LOOP('',(#8603,#8604,#8605,#8606));
#1987=EDGE_LOOP('',(#8607,#8608,#8609,#8610));
#1988=EDGE_LOOP('',(#8611,#8612,#8613,#8614));
#1989=EDGE_LOOP('',(#8615,#8616,#8617,#8618));
#1990=EDGE_LOOP('',(#8619,#8620,#8621,#8622));
#1991=EDGE_LOOP('',(#8623,#8624,#8625,#8626));
#1992=EDGE_LOOP('',(#8627,#8628,#8629,#8630));
#1993=EDGE_LOOP('',(#8631,#8632,#8633,#8634));
#1994=EDGE_LOOP('',(#8635,#8636,#8637,#8638));
#1995=EDGE_LOOP('',(#8639,#8640,#8641,#8642));
#1996=EDGE_LOOP('',(#8643,#8644,#8645,#8646));
#1997=EDGE_LOOP('',(#8647,#8648,#8649,#8650));
#1998=EDGE_LOOP('',(#8651,#8652,#8653,#8654));
#1999=EDGE_LOOP('',(#8655,#8656,#8657,#8658));
#2000=EDGE_LOOP('',(#8659,#8660,#8661,#8662));
#2001=EDGE_LOOP('',(#8663,#8664,#8665,#8666));
#2002=EDGE_LOOP('',(#8667,#8668,#8669,#8670));
#2003=EDGE_LOOP('',(#8671,#8672,#8673,#8674));
#2004=EDGE_LOOP('',(#8675,#8676,#8677,#8678));
#2005=EDGE_LOOP('',(#8679,#8680,#8681,#8682));
#2006=EDGE_LOOP('',(#8683,#8684,#8685,#8686));
#2007=EDGE_LOOP('',(#8687,#8688,#8689,#8690));
#2008=EDGE_LOOP('',(#8691,#8692,#8693,#8694));
#2009=EDGE_LOOP('',(#8695,#8696,#8697,#8698));
#2010=EDGE_LOOP('',(#8699,#8700,#8701,#8702));
#2011=EDGE_LOOP('',(#8703,#8704,#8705,#8706));
#2012=EDGE_LOOP('',(#8707,#8708,#8709,#8710));
#2013=EDGE_LOOP('',(#8711,#8712,#8713,#8714));
#2014=EDGE_LOOP('',(#8715,#8716,#8717,#8718));
#2015=EDGE_LOOP('',(#8719,#8720,#8721,#8722));
#2016=EDGE_LOOP('',(#8723,#8724,#8725,#8726));
#2017=EDGE_LOOP('',(#8727,#8728,#8729,#8730));
#2018=EDGE_LOOP('',(#8731,#8732,#8733,#8734));
#2019=EDGE_LOOP('',(#8735,#8736,#8737,#8738));
#2020=EDGE_LOOP('',(#8739,#8740,#8741,#8742));
#2021=EDGE_LOOP('',(#8743,#8744,#8745,#8746));
#2022=EDGE_LOOP('',(#8747,#8748,#8749,#8750));
#2023=EDGE_LOOP('',(#8751,#8752,#8753,#8754));
#2024=EDGE_LOOP('',(#8755,#8756,#8757,#8758));
#2025=EDGE_LOOP('',(#8759,#8760,#8761,#8762));
#2026=EDGE_LOOP('',(#8763,#8764,#8765,#8766));
#2027=EDGE_LOOP('',(#8767,#8768,#8769,#8770));
#2028=EDGE_LOOP('',(#8771,#8772,#8773,#8774));
#2029=EDGE_LOOP('',(#8775,#8776,#8777,#8778));
#2030=EDGE_LOOP('',(#8779,#8780,#8781,#8782));
#2031=EDGE_LOOP('',(#8783,#8784,#8785,#8786));
#2032=EDGE_LOOP('',(#8787,#8788,#8789,#8790));
#2033=EDGE_LOOP('',(#8791,#8792,#8793,#8794));
#2034=EDGE_LOOP('',(#8795,#8796,#8797,#8798));
#2035=EDGE_LOOP('',(#8799,#8800,#8801,#8802));
#2036=EDGE_LOOP('',(#8803,#8804,#8805,#8806));
#2037=EDGE_LOOP('',(#8807,#8808,#8809,#8810));
#2038=EDGE_LOOP('',(#8811,#8812,#8813,#8814));
#2039=EDGE_LOOP('',(#8815,#8816,#8817,#8818));
#2040=EDGE_LOOP('',(#8819,#8820,#8821,#8822));
#2041=EDGE_LOOP('',(#8823,#8824,#8825,#8826));
#2042=EDGE_LOOP('',(#8827,#8828,#8829,#8830));
#2043=EDGE_LOOP('',(#8831,#8832,#8833,#8834));
#2044=EDGE_LOOP('',(#8835,#8836,#8837,#8838));
#2045=EDGE_LOOP('',(#8839,#8840,#8841,#8842));
#2046=EDGE_LOOP('',(#8843,#8844,#8845,#8846));
#2047=EDGE_LOOP('',(#8847,#8848,#8849,#8850));
#2048=EDGE_LOOP('',(#8851,#8852,#8853,#8854));
#2049=EDGE_LOOP('',(#8855,#8856,#8857,#8858));
#2050=EDGE_LOOP('',(#8859,#8860,#8861,#8862));
#2051=EDGE_LOOP('',(#8863,#8864,#8865,#8866));
#2052=EDGE_LOOP('',(#8867,#8868,#8869,#8870,#8871,#8872,#8873,#8874,#8875,
#8876,#8877,#8878,#8879,#8880));
#2053=EDGE_LOOP('',(#8881));
#2054=EDGE_LOOP('',(#8882));
#2055=EDGE_LOOP('',(#8883,#8884,#8885,#8886,#8887,#8888,#8889,#8890,#8891,
#8892,#8893,#8894,#8895,#8896));
#2056=EDGE_LOOP('',(#8897));
#2057=EDGE_LOOP('',(#8898));
#2058=EDGE_LOOP('',(#8899,#8900,#8901,#8902));
#2059=EDGE_LOOP('',(#8903,#8904,#8905,#8906));
#2060=EDGE_LOOP('',(#8907,#8908,#8909,#8910));
#2061=EDGE_LOOP('',(#8911,#8912,#8913,#8914));
#2062=EDGE_LOOP('',(#8915,#8916,#8917,#8918));
#2063=EDGE_LOOP('',(#8919,#8920,#8921,#8922));
#2064=EDGE_LOOP('',(#8923,#8924,#8925,#8926));
#2065=EDGE_LOOP('',(#8927,#8928,#8929,#8930));
#2066=EDGE_LOOP('',(#8931,#8932,#8933,#8934));
#2067=EDGE_LOOP('',(#8935,#8936,#8937,#8938));
#2068=EDGE_LOOP('',(#8939,#8940,#8941,#8942));
#2069=EDGE_LOOP('',(#8943,#8944,#8945,#8946));
#2070=EDGE_LOOP('',(#8947,#8948,#8949,#8950));
#2071=EDGE_LOOP('',(#8951,#8952,#8953,#8954));
#2072=EDGE_LOOP('',(#8955,#8956,#8957,#8958));
#2073=EDGE_LOOP('',(#8959,#8960,#8961,#8962,#8963));
#2074=EDGE_LOOP('',(#8964,#8965,#8966,#8967,#8968));
#2075=EDGE_LOOP('',(#8969,#8970,#8971,#8972));
#2076=EDGE_LOOP('',(#8973));
#2077=EDGE_LOOP('',(#8974));
#2078=EDGE_LOOP('',(#8975));
#2079=EDGE_LOOP('',(#8976));
#2080=EDGE_LOOP('',(#8977,#8978,#8979,#8980));
#2081=EDGE_LOOP('',(#8981,#8982,#8983,#8984));
#2082=EDGE_LOOP('',(#8985));
#2083=EDGE_LOOP('',(#8986));
#2084=EDGE_LOOP('',(#8987));
#2085=EDGE_LOOP('',(#8988));
#2086=EDGE_LOOP('',(#8989,#8990,#8991,#8992));
#2087=EDGE_LOOP('',(#8993,#8994,#8995,#8996,#8997,#8998));
#2088=EDGE_LOOP('',(#8999));
#2089=EDGE_LOOP('',(#9000,#9001,#9002,#9003,#9004,#9005));
#2090=EDGE_LOOP('',(#9006));
#2091=EDGE_LOOP('',(#9007,#9008,#9009,#9010));
#2092=EDGE_LOOP('',(#9011,#9012,#9013,#9014));
#2093=EDGE_LOOP('',(#9015,#9016,#9017,#9018));
#2094=EDGE_LOOP('',(#9019,#9020,#9021,#9022));
#2095=EDGE_LOOP('',(#9023,#9024,#9025,#9026));
#2096=EDGE_LOOP('',(#9027,#9028,#9029,#9030));
#2097=EDGE_LOOP('',(#9031,#9032,#9033,#9034));
#2098=EDGE_LOOP('',(#9035,#9036,#9037,#9038));
#2099=EDGE_LOOP('',(#9039));
#2100=EDGE_LOOP('',(#9040,#9041,#9042,#9043,#9044,#9045));
#2101=EDGE_LOOP('',(#9046));
#2102=EDGE_LOOP('',(#9047));
#2103=EDGE_LOOP('',(#9048));
#2104=EDGE_LOOP('',(#9049,#9050,#9051,#9052));
#2105=EDGE_LOOP('',(#9053,#9054,#9055,#9056));
#2106=EDGE_LOOP('',(#9057,#9058,#9059,#9060));
#2107=EDGE_LOOP('',(#9061,#9062,#9063,#9064));
#2108=EDGE_LOOP('',(#9065,#9066,#9067,#9068));
#2109=EDGE_LOOP('',(#9069,#9070,#9071,#9072));
#2110=EDGE_LOOP('',(#9073,#9074,#9075,#9076,#9077,#9078));
#2111=EDGE_LOOP('',(#9079,#9080,#9081,#9082));
#2112=EDGE_LOOP('',(#9083,#9084,#9085,#9086));
#2113=EDGE_LOOP('',(#9087,#9088,#9089,#9090));
#2114=EDGE_LOOP('',(#9091,#9092,#9093,#9094));
#2115=EDGE_LOOP('',(#9095,#9096,#9097,#9098));
#2116=EDGE_LOOP('',(#9099,#9100,#9101,#9102));
#2117=EDGE_LOOP('',(#9103,#9104,#9105,#9106));
#2118=EDGE_LOOP('',(#9107,#9108,#9109,#9110,#9111,#9112));
#2119=EDGE_LOOP('',(#9113));
#2120=EDGE_LOOP('',(#9114,#9115,#9116,#9117,#9118,#9119));
#2121=EDGE_LOOP('',(#9120));
#2122=EDGE_LOOP('',(#9121,#9122,#9123,#9124));
#2123=EDGE_LOOP('',(#9125,#9126,#9127,#9128));
#2124=EDGE_LOOP('',(#9129));
#2125=EDGE_LOOP('',(#9130,#9131,#9132,#9133,#9134,#9135));
#2126=EDGE_LOOP('',(#9136));
#2127=EDGE_LOOP('',(#9137));
#2128=EDGE_LOOP('',(#9138));
#2129=EDGE_LOOP('',(#9139,#9140,#9141,#9142));
#2130=EDGE_LOOP('',(#9143,#9144,#9145,#9146));
#2131=EDGE_LOOP('',(#9147,#9148,#9149,#9150));
#2132=EDGE_LOOP('',(#9151,#9152,#9153,#9154));
#2133=EDGE_LOOP('',(#9155,#9156,#9157,#9158));
#2134=EDGE_LOOP('',(#9159,#9160,#9161,#9162));
#2135=EDGE_LOOP('',(#9163,#9164,#9165,#9166,#9167,#9168));
#2136=LINE('',#13686,#3184);
#2137=LINE('',#13692,#3185);
#2138=LINE('',#13697,#3186);
#2139=LINE('',#13699,#3187);
#2140=LINE('',#13701,#3188);
#2141=LINE('',#13703,#3189);
#2142=LINE('',#13705,#3190);
#2143=LINE('',#13707,#3191);
#2144=LINE('',#13709,#3192);
#2145=LINE('',#13711,#3193);
#2146=LINE('',#13713,#3194);
#2147=LINE('',#13715,#3195);
#2148=LINE('',#13717,#3196);
#2149=LINE('',#13719,#3197);
#2150=LINE('',#13721,#3198);
#2151=LINE('',#13723,#3199);
#2152=LINE('',#13725,#3200);
#2153=LINE('',#13727,#3201);
#2154=LINE('',#13729,#3202);
#2155=LINE('',#13731,#3203);
#2156=LINE('',#13733,#3204);
#2157=LINE('',#13735,#3205);
#2158=LINE('',#13737,#3206);
#2159=LINE('',#13739,#3207);
#2160=LINE('',#13741,#3208);
#2161=LINE('',#13743,#3209);
#2162=LINE('',#13745,#3210);
#2163=LINE('',#13747,#3211);
#2164=LINE('',#13749,#3212);
#2165=LINE('',#13751,#3213);
#2166=LINE('',#13753,#3214);
#2167=LINE('',#13755,#3215);
#2168=LINE('',#13757,#3216);
#2169=LINE('',#13758,#3217);
#2170=LINE('',#13761,#3218);
#2171=LINE('',#13763,#3219);
#2172=LINE('',#13765,#3220);
#2173=LINE('',#13766,#3221);
#2174=LINE('',#13769,#3222);
#2175=LINE('',#13771,#3223);
#2176=LINE('',#13773,#3224);
#2177=LINE('',#13774,#3225);
#2178=LINE('',#13777,#3226);
#2179=LINE('',#13779,#3227);
#2180=LINE('',#13780,#3228);
#2181=LINE('',#13783,#3229);
#2182=LINE('',#13785,#3230);
#2183=LINE('',#13786,#3231);
#2184=LINE('',#13789,#3232);
#2185=LINE('',#13791,#3233);
#2186=LINE('',#13792,#3234);
#2187=LINE('',#13795,#3235);
#2188=LINE('',#13797,#3236);
#2189=LINE('',#13798,#3237);
#2190=LINE('',#13801,#3238);
#2191=LINE('',#13803,#3239);
#2192=LINE('',#13804,#3240);
#2193=LINE('',#13807,#3241);
#2194=LINE('',#13809,#3242);
#2195=LINE('',#13810,#3243);
#2196=LINE('',#13813,#3244);
#2197=LINE('',#13815,#3245);
#2198=LINE('',#13816,#3246);
#2199=LINE('',#13819,#3247);
#2200=LINE('',#13821,#3248);
#2201=LINE('',#13822,#3249);
#2202=LINE('',#13825,#3250);
#2203=LINE('',#13827,#3251);
#2204=LINE('',#13828,#3252);
#2205=LINE('',#13830,#3253);
#2206=LINE('',#13832,#3254);
#2207=LINE('',#13833,#3255);
#2208=LINE('',#13835,#3256);
#2209=LINE('',#13837,#3257);
#2210=LINE('',#13838,#3258);
#2211=LINE('',#13839,#3259);
#2212=LINE('',#13841,#3260);
#2213=LINE('',#13843,#3261);
#2214=LINE('',#13844,#3262);
#2215=LINE('',#13846,#3263);
#2216=LINE('',#13848,#3264);
#2217=LINE('',#13849,#3265);
#2218=LINE('',#13851,#3266);
#2219=LINE('',#13853,#3267);
#2220=LINE('',#13854,#3268);
#2221=LINE('',#13855,#3269);
#2222=LINE('',#13861,#3270);
#2223=LINE('',#13863,#3271);
#2224=LINE('',#13864,#3272);
#2225=LINE('',#13867,#3273);
#2226=LINE('',#13869,#3274);
#2227=LINE('',#13870,#3275);
#2228=LINE('',#13873,#3276);
#2229=LINE('',#13875,#3277);
#2230=LINE('',#13876,#3278);
#2231=LINE('',#13878,#3279);
#2232=LINE('',#13879,#3280);
#2233=LINE('',#13884,#3281);
#2234=LINE('',#13886,#3282);
#2235=LINE('',#13887,#3283);
#2236=LINE('',#13890,#3284);
#2237=LINE('',#13892,#3285);
#2238=LINE('',#13893,#3286);
#2239=LINE('',#13896,#3287);
#2240=LINE('',#13898,#3288);
#2241=LINE('',#13899,#3289);
#2242=LINE('',#13901,#3290);
#2243=LINE('',#13902,#3291);
#2244=LINE('',#13906,#3292);
#2245=LINE('',#13908,#3293);
#2246=LINE('',#13911,#3294);
#2247=LINE('',#13913,#3295);
#2248=LINE('',#13916,#3296);
#2249=LINE('',#13918,#3297);
#2250=LINE('',#13921,#3298);
#2251=LINE('',#13923,#3299);
#2252=LINE('',#13926,#3300);
#2253=LINE('',#13928,#3301);
#2254=LINE('',#13931,#3302);
#2255=LINE('',#13933,#3303);
#2256=LINE('',#13946,#3304);
#2257=LINE('',#13949,#3305);
#2258=LINE('',#13954,#3306);
#2259=LINE('',#13960,#3307);
#2260=LINE('',#13966,#3308);
#2261=LINE('',#13976,#3309);
#2262=LINE('',#13986,#3310);
#2263=LINE('',#13993,#3311);
#2264=LINE('',#13995,#3312);
#2265=LINE('',#13997,#3313);
#2266=LINE('',#13999,#3314);
#2267=LINE('',#14001,#3315);
#2268=LINE('',#14002,#3316);
#2269=LINE('',#14005,#3317);
#2270=LINE('',#14007,#3318);
#2271=LINE('',#14009,#3319);
#2272=LINE('',#14010,#3320);
#2273=LINE('',#14013,#3321);
#2274=LINE('',#14015,#3322);
#2275=LINE('',#14017,#3323);
#2276=LINE('',#14018,#3324);
#2277=LINE('',#14022,#3325);
#2278=LINE('',#14024,#3326);
#2279=LINE('',#14026,#3327);
#2280=LINE('',#14027,#3328);
#2281=LINE('',#14028,#3329);
#2282=LINE('',#14029,#3330);
#2283=LINE('',#14030,#3331);
#2284=LINE('',#14033,#3332);
#2285=LINE('',#14035,#3333);
#2286=LINE('',#14036,#3334);
#2287=LINE('',#14039,#3335);
#2288=LINE('',#14041,#3336);
#2289=LINE('',#14042,#3337);
#2290=LINE('',#14045,#3338);
#2291=LINE('',#14047,#3339);
#2292=LINE('',#14048,#3340);
#2293=LINE('',#14051,#3341);
#2294=LINE('',#14053,#3342);
#2295=LINE('',#14054,#3343);
#2296=LINE('',#14057,#3344);
#2297=LINE('',#14059,#3345);
#2298=LINE('',#14060,#3346);
#2299=LINE('',#14062,#3347);
#2300=LINE('',#14063,#3348);
#2301=LINE('',#14066,#3349);
#2302=LINE('',#14068,#3350);
#2303=LINE('',#14069,#3351);
#2304=LINE('',#14072,#3352);
#2305=LINE('',#14074,#3353);
#2306=LINE('',#14075,#3354);
#2307=LINE('',#14078,#3355);
#2308=LINE('',#14080,#3356);
#2309=LINE('',#14081,#3357);
#2310=LINE('',#14083,#3358);
#2311=LINE('',#14084,#3359);
#2312=LINE('',#14089,#3360);
#2313=LINE('',#14091,#3361);
#2314=LINE('',#14092,#3362);
#2315=LINE('',#14095,#3363);
#2316=LINE('',#14097,#3364);
#2317=LINE('',#14098,#3365);
#2318=LINE('',#14101,#3366);
#2319=LINE('',#14103,#3367);
#2320=LINE('',#14104,#3368);
#2321=LINE('',#14106,#3369);
#2322=LINE('',#14107,#3370);
#2323=LINE('',#14112,#3371);
#2324=LINE('',#14114,#3372);
#2325=LINE('',#14115,#3373);
#2326=LINE('',#14118,#3374);
#2327=LINE('',#14120,#3375);
#2328=LINE('',#14121,#3376);
#2329=LINE('',#14124,#3377);
#2330=LINE('',#14126,#3378);
#2331=LINE('',#14127,#3379);
#2332=LINE('',#14129,#3380);
#2333=LINE('',#14130,#3381);
#2334=LINE('',#14144,#3382);
#2335=LINE('',#14154,#3383);
#2336=LINE('',#14164,#3384);
#2337=LINE('',#14174,#3385);
#2338=LINE('',#14180,#3386);
#2339=LINE('',#14186,#3387);
#2340=LINE('',#14191,#3388);
#2341=LINE('',#14193,#3389);
#2342=LINE('',#14195,#3390);
#2343=LINE('',#14197,#3391);
#2344=LINE('',#14199,#3392);
#2345=LINE('',#14201,#3393);
#2346=LINE('',#14203,#3394);
#2347=LINE('',#14205,#3395);
#2348=LINE('',#14207,#3396);
#2349=LINE('',#14209,#3397);
#2350=LINE('',#14211,#3398);
#2351=LINE('',#14212,#3399);
#2352=LINE('',#14215,#3400);
#2353=LINE('',#14217,#3401);
#2354=LINE('',#14219,#3402);
#2355=LINE('',#14221,#3403);
#2356=LINE('',#14223,#3404);
#2357=LINE('',#14225,#3405);
#2358=LINE('',#14227,#3406);
#2359=LINE('',#14229,#3407);
#2360=LINE('',#14231,#3408);
#2361=LINE('',#14233,#3409);
#2362=LINE('',#14235,#3410);
#2363=LINE('',#14236,#3411);
#2364=LINE('',#14240,#3412);
#2365=LINE('',#14242,#3413);
#2366=LINE('',#14244,#3414);
#2367=LINE('',#14246,#3415);
#2368=LINE('',#14248,#3416);
#2369=LINE('',#14250,#3417);
#2370=LINE('',#14252,#3418);
#2371=LINE('',#14254,#3419);
#2372=LINE('',#14256,#3420);
#2373=LINE('',#14258,#3421);
#2374=LINE('',#14260,#3422);
#2375=LINE('',#14261,#3423);
#2376=LINE('',#14264,#3424);
#2377=LINE('',#14266,#3425);
#2378=LINE('',#14267,#3426);
#2379=LINE('',#14269,#3427);
#2380=LINE('',#14271,#3428);
#2381=LINE('',#14272,#3429);
#2382=LINE('',#14275,#3430);
#2383=LINE('',#14277,#3431);
#2384=LINE('',#14278,#3432);
#2385=LINE('',#14282,#3433);
#2386=LINE('',#14283,#3434);
#2387=LINE('',#14284,#3435);
#2388=LINE('',#14288,#3436);
#2389=LINE('',#14289,#3437);
#2390=LINE('',#14290,#3438);
#2391=LINE('',#14293,#3439);
#2392=LINE('',#14295,#3440);
#2393=LINE('',#14296,#3441);
#2394=LINE('',#14299,#3442);
#2395=LINE('',#14301,#3443);
#2396=LINE('',#14302,#3444);
#2397=LINE('',#14306,#3445);
#2398=LINE('',#14307,#3446);
#2399=LINE('',#14308,#3447);
#2400=LINE('',#14312,#3448);
#2401=LINE('',#14314,#3449);
#2402=LINE('',#14316,#3450);
#2403=LINE('',#14317,#3451);
#2404=LINE('',#14321,#3452);
#2405=LINE('',#14323,#3453);
#2406=LINE('',#14325,#3454);
#2407=LINE('',#14326,#3455);
#2408=LINE('',#14330,#3456);
#2409=LINE('',#14331,#3457);
#2410=LINE('',#14332,#3458);
#2411=LINE('',#14335,#3459);
#2412=LINE('',#14337,#3460);
#2413=LINE('',#14338,#3461);
#2414=LINE('',#14341,#3462);
#2415=LINE('',#14343,#3463);
#2416=LINE('',#14344,#3464);
#2417=LINE('',#14345,#3465);
#2418=LINE('',#14346,#3466);
#2419=LINE('',#14347,#3467);
#2420=LINE('',#14351,#3468);
#2421=LINE('',#14353,#3469);
#2422=LINE('',#14354,#3470);
#2423=LINE('',#14355,#3471);
#2424=LINE('',#14356,#3472);
#2425=LINE('',#14358,#3473);
#2426=LINE('',#14361,#3474);
#2427=LINE('',#14362,#3475);
#2428=LINE('',#14365,#3476);
#2429=LINE('',#14366,#3477);
#2430=LINE('',#14369,#3478);
#2431=LINE('',#14370,#3479);
#2432=LINE('',#14372,#3480);
#2433=LINE('',#14374,#3481);
#2434=LINE('',#14376,#3482);
#2435=LINE('',#14377,#3483);
#2436=LINE('',#14379,#3484);
#2437=LINE('',#14382,#3485);
#2438=LINE('',#14384,#3486);
#2439=LINE('',#14386,#3487);
#2440=LINE('',#14388,#3488);
#2441=LINE('',#14389,#3489);
#2442=LINE('',#14391,#3490);
#2443=LINE('',#14394,#3491);
#2444=LINE('',#14396,#3492);
#2445=LINE('',#14398,#3493);
#2446=LINE('',#14400,#3494);
#2447=LINE('',#14401,#3495);
#2448=LINE('',#14404,#3496);
#2449=LINE('',#14405,#3497);
#2450=LINE('',#14408,#3498);
#2451=LINE('',#14409,#3499);
#2452=LINE('',#14412,#3500);
#2453=LINE('',#14413,#3501);
#2454=LINE('',#14416,#3502);
#2455=LINE('',#14417,#3503);
#2456=LINE('',#14419,#3504);
#2457=LINE('',#14423,#3505);
#2458=LINE('',#14424,#3506);
#2459=LINE('',#14427,#3507);
#2460=LINE('',#14428,#3508);
#2461=LINE('',#14431,#3509);
#2462=LINE('',#14432,#3510);
#2463=LINE('',#14435,#3511);
#2464=LINE('',#14436,#3512);
#2465=LINE('',#14438,#3513);
#2466=LINE('',#14441,#3514);
#2467=LINE('',#14442,#3515);
#2468=LINE('',#14444,#3516);
#2469=LINE('',#14445,#3517);
#2470=LINE('',#14447,#3518);
#2471=LINE('',#14448,#3519);
#2472=LINE('',#14449,#3520);
#2473=LINE('',#14451,#3521);
#2474=LINE('',#14452,#3522);
#2475=LINE('',#14454,#3523);
#2476=LINE('',#14455,#3524);
#2477=LINE('',#14457,#3525);
#2478=LINE('',#14458,#3526);
#2479=LINE('',#14459,#3527);
#2480=LINE('',#14468,#3528);
#2481=LINE('',#14478,#3529);
#2482=LINE('',#14484,#3530);
#2483=LINE('',#14490,#3531);
#2484=LINE('',#14496,#3532);
#2485=LINE('',#14502,#3533);
#2486=LINE('',#14507,#3534);
#2487=LINE('',#14509,#3535);
#2488=LINE('',#14511,#3536);
#2489=LINE('',#14512,#3537);
#2490=LINE('',#14516,#3538);
#2491=LINE('',#14518,#3539);
#2492=LINE('',#14520,#3540);
#2493=LINE('',#14521,#3541);
#2494=LINE('',#14524,#3542);
#2495=LINE('',#14526,#3543);
#2496=LINE('',#14527,#3544);
#2497=LINE('',#14530,#3545);
#2498=LINE('',#14532,#3546);
#2499=LINE('',#14533,#3547);
#2500=LINE('',#14536,#3548);
#2501=LINE('',#14538,#3549);
#2502=LINE('',#14539,#3550);
#2503=LINE('',#14542,#3551);
#2504=LINE('',#14544,#3552);
#2505=LINE('',#14545,#3553);
#2506=LINE('',#14547,#3554);
#2507=LINE('',#14548,#3555);
#2508=LINE('',#14551,#3556);
#2509=LINE('',#14553,#3557);
#2510=LINE('',#14554,#3558);
#2511=LINE('',#14557,#3559);
#2512=LINE('',#14559,#3560);
#2513=LINE('',#14560,#3561);
#2514=LINE('',#14562,#3562);
#2515=LINE('',#14564,#3563);
#2516=LINE('',#14575,#3564);
#2517=LINE('',#14577,#3565);
#2518=LINE('',#14579,#3566);
#2519=LINE('',#14580,#3567);
#2520=LINE('',#14583,#3568);
#2521=LINE('',#14585,#3569);
#2522=LINE('',#14586,#3570);
#2523=LINE('',#14589,#3571);
#2524=LINE('',#14591,#3572);
#2525=LINE('',#14592,#3573);
#2526=LINE('',#14594,#3574);
#2527=LINE('',#14595,#3575);
#2528=LINE('',#14602,#3576);
#2529=LINE('',#14604,#3577);
#2530=LINE('',#14606,#3578);
#2531=LINE('',#14607,#3579);
#2532=LINE('',#14610,#3580);
#2533=LINE('',#14612,#3581);
#2534=LINE('',#14613,#3582);
#2535=LINE('',#14616,#3583);
#2536=LINE('',#14618,#3584);
#2537=LINE('',#14619,#3585);
#2538=LINE('',#14621,#3586);
#2539=LINE('',#14622,#3587);
#2540=LINE('',#14630,#3588);
#2541=LINE('',#14636,#3589);
#2542=LINE('',#14642,#3590);
#2543=LINE('',#14648,#3591);
#2544=LINE('',#14653,#3592);
#2545=LINE('',#14655,#3593);
#2546=LINE('',#14657,#3594);
#2547=LINE('',#14658,#3595);
#2548=LINE('',#14661,#3596);
#2549=LINE('',#14663,#3597);
#2550=LINE('',#14664,#3598);
#2551=LINE('',#14667,#3599);
#2552=LINE('',#14669,#3600);
#2553=LINE('',#14670,#3601);
#2554=LINE('',#14672,#3602);
#2555=LINE('',#14673,#3603);
#2556=LINE('',#14683,#3604);
#2557=LINE('',#14689,#3605);
#2558=LINE('',#14695,#3606);
#2559=LINE('',#14701,#3607);
#2560=LINE('',#14707,#3608);
#2561=LINE('',#14720,#3609);
#2562=LINE('',#14726,#3610);
#2563=LINE('',#14732,#3611);
#2564=LINE('',#14738,#3612);
#2565=LINE('',#14744,#3613);
#2566=LINE('',#14757,#3614);
#2567=LINE('',#14818,#3615);
#2568=LINE('',#14843,#3616);
#2569=LINE('',#14849,#3617);
#2570=LINE('',#14856,#3618);
#2571=LINE('',#14860,#3619);
#2572=LINE('',#14863,#3620);
#2573=LINE('',#14865,#3621);
#2574=LINE('',#14870,#3622);
#2575=LINE('',#14873,#3623);
#2576=LINE('',#14875,#3624);
#2577=LINE('',#14877,#3625);
#2578=LINE('',#14882,#3626);
#2579=LINE('',#14884,#3627);
#2580=LINE('',#14891,#3628);
#2581=LINE('',#14896,#3629);
#2582=LINE('',#14898,#3630);
#2583=LINE('',#14900,#3631);
#2584=LINE('',#14901,#3632);
#2585=LINE('',#14905,#3633);
#2586=LINE('',#14907,#3634);
#2587=LINE('',#14909,#3635);
#2588=LINE('',#14910,#3636);
#2589=LINE('',#14912,#3637);
#2590=LINE('',#14913,#3638);
#2591=LINE('',#14915,#3639);
#2592=LINE('',#14917,#3640);
#2593=LINE('',#14924,#3641);
#2594=LINE('',#14929,#3642);
#2595=LINE('',#14931,#3643);
#2596=LINE('',#14933,#3644);
#2597=LINE('',#14934,#3645);
#2598=LINE('',#14938,#3646);
#2599=LINE('',#14940,#3647);
#2600=LINE('',#14942,#3648);
#2601=LINE('',#14943,#3649);
#2602=LINE('',#14945,#3650);
#2603=LINE('',#14946,#3651);
#2604=LINE('',#14948,#3652);
#2605=LINE('',#14950,#3653);
#2606=LINE('',#14957,#3654);
#2607=LINE('',#15005,#3655);
#2608=LINE('',#15010,#3656);
#2609=LINE('',#15020,#3657);
#2610=LINE('',#15029,#3658);
#2611=LINE('',#15035,#3659);
#2612=LINE('',#15041,#3660);
#2613=LINE('',#15047,#3661);
#2614=LINE('',#15052,#3662);
#2615=LINE('',#15054,#3663);
#2616=LINE('',#15056,#3664);
#2617=LINE('',#15057,#3665);
#2618=LINE('',#15060,#3666);
#2619=LINE('',#15062,#3667);
#2620=LINE('',#15063,#3668);
#2621=LINE('',#15066,#3669);
#2622=LINE('',#15068,#3670);
#2623=LINE('',#15069,#3671);
#2624=LINE('',#15071,#3672);
#2625=LINE('',#15072,#3673);
#2626=LINE('',#15082,#3674);
#2627=LINE('',#15088,#3675);
#2628=LINE('',#15094,#3676);
#2629=LINE('',#15099,#3677);
#2630=LINE('',#15101,#3678);
#2631=LINE('',#15103,#3679);
#2632=LINE('',#15105,#3680);
#2633=LINE('',#15107,#3681);
#2634=LINE('',#15109,#3682);
#2635=LINE('',#15111,#3683);
#2636=LINE('',#15112,#3684);
#2637=LINE('',#15116,#3685);
#2638=LINE('',#15118,#3686);
#2639=LINE('',#15120,#3687);
#2640=LINE('',#15122,#3688);
#2641=LINE('',#15124,#3689);
#2642=LINE('',#15126,#3690);
#2643=LINE('',#15128,#3691);
#2644=LINE('',#15129,#3692);
#2645=LINE('',#15131,#3693);
#2646=LINE('',#15132,#3694);
#2647=LINE('',#15134,#3695);
#2648=LINE('',#15136,#3696);
#2649=LINE('',#15138,#3697);
#2650=LINE('',#15140,#3698);
#2651=LINE('',#15142,#3699);
#2652=LINE('',#15144,#3700);
#2653=LINE('',#15151,#3701);
#2654=LINE('',#15157,#3702);
#2655=LINE('',#15161,#3703);
#2656=LINE('',#15165,#3704);
#2657=LINE('',#15170,#3705);
#2658=LINE('',#15176,#3706);
#2659=LINE('',#15179,#3707);
#2660=LINE('',#15182,#3708);
#2661=LINE('',#15186,#3709);
#2662=LINE('',#15190,#3710);
#2663=LINE('',#15194,#3711);
#2664=LINE('',#15198,#3712);
#2665=LINE('',#15202,#3713);
#2666=LINE('',#15206,#3714);
#2667=LINE('',#15210,#3715);
#2668=LINE('',#15214,#3716);
#2669=LINE('',#15218,#3717);
#2670=LINE('',#15222,#3718);
#2671=LINE('',#15226,#3719);
#2672=LINE('',#15230,#3720);
#2673=LINE('',#15234,#3721);
#2674=LINE('',#15238,#3722);
#2675=LINE('',#15242,#3723);
#2676=LINE('',#15246,#3724);
#2677=LINE('',#15250,#3725);
#2678=LINE('',#15254,#3726);
#2679=LINE('',#15258,#3727);
#2680=LINE('',#15262,#3728);
#2681=LINE('',#15266,#3729);
#2682=LINE('',#15270,#3730);
#2683=LINE('',#15274,#3731);
#2684=LINE('',#15278,#3732);
#2685=LINE('',#15282,#3733);
#2686=LINE('',#15286,#3734);
#2687=LINE('',#15290,#3735);
#2688=LINE('',#15294,#3736);
#2689=LINE('',#15298,#3737);
#2690=LINE('',#15302,#3738);
#2691=LINE('',#15306,#3739);
#2692=LINE('',#15310,#3740);
#2693=LINE('',#15314,#3741);
#2694=LINE('',#15318,#3742);
#2695=LINE('',#15322,#3743);
#2696=LINE('',#15326,#3744);
#2697=LINE('',#15330,#3745);
#2698=LINE('',#15334,#3746);
#2699=LINE('',#15338,#3747);
#2700=LINE('',#15342,#3748);
#2701=LINE('',#15346,#3749);
#2702=LINE('',#15350,#3750);
#2703=LINE('',#15354,#3751);
#2704=LINE('',#15358,#3752);
#2705=LINE('',#15362,#3753);
#2706=LINE('',#15366,#3754);
#2707=LINE('',#15370,#3755);
#2708=LINE('',#15374,#3756);
#2709=LINE('',#15378,#3757);
#2710=LINE('',#15382,#3758);
#2711=LINE('',#15386,#3759);
#2712=LINE('',#15390,#3760);
#2713=LINE('',#15394,#3761);
#2714=LINE('',#15398,#3762);
#2715=LINE('',#15402,#3763);
#2716=LINE('',#15406,#3764);
#2717=LINE('',#15410,#3765);
#2718=LINE('',#15414,#3766);
#2719=LINE('',#15418,#3767);
#2720=LINE('',#15422,#3768);
#2721=LINE('',#15426,#3769);
#2722=LINE('',#15430,#3770);
#2723=LINE('',#15434,#3771);
#2724=LINE('',#15438,#3772);
#2725=LINE('',#15442,#3773);
#2726=LINE('',#15446,#3774);
#2727=LINE('',#15450,#3775);
#2728=LINE('',#15454,#3776);
#2729=LINE('',#15458,#3777);
#2730=LINE('',#15462,#3778);
#2731=LINE('',#15466,#3779);
#2732=LINE('',#15470,#3780);
#2733=LINE('',#15474,#3781);
#2734=LINE('',#15478,#3782);
#2735=LINE('',#15482,#3783);
#2736=LINE('',#15488,#3784);
#2737=LINE('',#15490,#3785);
#2738=LINE('',#15491,#3786);
#2739=LINE('',#15494,#3787);
#2740=LINE('',#15496,#3788);
#2741=LINE('',#15497,#3789);
#2742=LINE('',#15499,#3790);
#2743=LINE('',#15501,#3791);
#2744=LINE('',#15505,#3792);
#2745=LINE('',#15507,#3793);
#2746=LINE('',#15508,#3794);
#2747=LINE('',#15511,#3795);
#2748=LINE('',#15513,#3796);
#2749=LINE('',#15514,#3797);
#2750=LINE('',#15516,#3798);
#2751=LINE('',#15518,#3799);
#2752=LINE('',#15522,#3800);
#2753=LINE('',#15524,#3801);
#2754=LINE('',#15525,#3802);
#2755=LINE('',#15528,#3803);
#2756=LINE('',#15530,#3804);
#2757=LINE('',#15531,#3805);
#2758=LINE('',#15533,#3806);
#2759=LINE('',#15535,#3807);
#2760=LINE('',#15539,#3808);
#2761=LINE('',#15541,#3809);
#2762=LINE('',#15542,#3810);
#2763=LINE('',#15545,#3811);
#2764=LINE('',#15547,#3812);
#2765=LINE('',#15548,#3813);
#2766=LINE('',#15550,#3814);
#2767=LINE('',#15552,#3815);
#2768=LINE('',#15556,#3816);
#2769=LINE('',#15558,#3817);
#2770=LINE('',#15559,#3818);
#2771=LINE('',#15562,#3819);
#2772=LINE('',#15564,#3820);
#2773=LINE('',#15565,#3821);
#2774=LINE('',#15567,#3822);
#2775=LINE('',#15569,#3823);
#2776=LINE('',#15573,#3824);
#2777=LINE('',#15575,#3825);
#2778=LINE('',#15576,#3826);
#2779=LINE('',#15579,#3827);
#2780=LINE('',#15581,#3828);
#2781=LINE('',#15582,#3829);
#2782=LINE('',#15584,#3830);
#2783=LINE('',#15586,#3831);
#2784=LINE('',#15590,#3832);
#2785=LINE('',#15592,#3833);
#2786=LINE('',#15593,#3834);
#2787=LINE('',#15596,#3835);
#2788=LINE('',#15598,#3836);
#2789=LINE('',#15599,#3837);
#2790=LINE('',#15601,#3838);
#2791=LINE('',#15603,#3839);
#2792=LINE('',#15607,#3840);
#2793=LINE('',#15609,#3841);
#2794=LINE('',#15610,#3842);
#2795=LINE('',#15613,#3843);
#2796=LINE('',#15615,#3844);
#2797=LINE('',#15616,#3845);
#2798=LINE('',#15618,#3846);
#2799=LINE('',#15620,#3847);
#2800=LINE('',#15624,#3848);
#2801=LINE('',#15626,#3849);
#2802=LINE('',#15627,#3850);
#2803=LINE('',#15630,#3851);
#2804=LINE('',#15632,#3852);
#2805=LINE('',#15633,#3853);
#2806=LINE('',#15635,#3854);
#2807=LINE('',#15637,#3855);
#2808=LINE('',#15641,#3856);
#2809=LINE('',#15643,#3857);
#2810=LINE('',#15644,#3858);
#2811=LINE('',#15647,#3859);
#2812=LINE('',#15649,#3860);
#2813=LINE('',#15650,#3861);
#2814=LINE('',#15652,#3862);
#2815=LINE('',#15654,#3863);
#2816=LINE('',#15658,#3864);
#2817=LINE('',#15660,#3865);
#2818=LINE('',#15661,#3866);
#2819=LINE('',#15664,#3867);
#2820=LINE('',#15666,#3868);
#2821=LINE('',#15667,#3869);
#2822=LINE('',#15669,#3870);
#2823=LINE('',#15671,#3871);
#2824=LINE('',#15675,#3872);
#2825=LINE('',#15677,#3873);
#2826=LINE('',#15678,#3874);
#2827=LINE('',#15681,#3875);
#2828=LINE('',#15683,#3876);
#2829=LINE('',#15684,#3877);
#2830=LINE('',#15686,#3878);
#2831=LINE('',#15688,#3879);
#2832=LINE('',#15692,#3880);
#2833=LINE('',#15694,#3881);
#2834=LINE('',#15695,#3882);
#2835=LINE('',#15698,#3883);
#2836=LINE('',#15700,#3884);
#2837=LINE('',#15701,#3885);
#2838=LINE('',#15703,#3886);
#2839=LINE('',#15705,#3887);
#2840=LINE('',#15709,#3888);
#2841=LINE('',#15711,#3889);
#2842=LINE('',#15712,#3890);
#2843=LINE('',#15715,#3891);
#2844=LINE('',#15717,#3892);
#2845=LINE('',#15718,#3893);
#2846=LINE('',#15720,#3894);
#2847=LINE('',#15722,#3895);
#2848=LINE('',#15726,#3896);
#2849=LINE('',#15728,#3897);
#2850=LINE('',#15729,#3898);
#2851=LINE('',#15732,#3899);
#2852=LINE('',#15734,#3900);
#2853=LINE('',#15735,#3901);
#2854=LINE('',#15737,#3902);
#2855=LINE('',#15739,#3903);
#2856=LINE('',#15743,#3904);
#2857=LINE('',#15745,#3905);
#2858=LINE('',#15746,#3906);
#2859=LINE('',#15749,#3907);
#2860=LINE('',#15751,#3908);
#2861=LINE('',#15752,#3909);
#2862=LINE('',#15754,#3910);
#2863=LINE('',#15756,#3911);
#2864=LINE('',#15760,#3912);
#2865=LINE('',#15762,#3913);
#2866=LINE('',#15763,#3914);
#2867=LINE('',#15766,#3915);
#2868=LINE('',#15768,#3916);
#2869=LINE('',#15769,#3917);
#2870=LINE('',#15771,#3918);
#2871=LINE('',#15773,#3919);
#2872=LINE('',#15777,#3920);
#2873=LINE('',#15779,#3921);
#2874=LINE('',#15780,#3922);
#2875=LINE('',#15783,#3923);
#2876=LINE('',#15785,#3924);
#2877=LINE('',#15786,#3925);
#2878=LINE('',#15788,#3926);
#2879=LINE('',#15790,#3927);
#2880=LINE('',#15794,#3928);
#2881=LINE('',#15796,#3929);
#2882=LINE('',#15797,#3930);
#2883=LINE('',#15800,#3931);
#2884=LINE('',#15802,#3932);
#2885=LINE('',#15803,#3933);
#2886=LINE('',#15805,#3934);
#2887=LINE('',#15807,#3935);
#2888=LINE('',#15811,#3936);
#2889=LINE('',#15813,#3937);
#2890=LINE('',#15814,#3938);
#2891=LINE('',#15817,#3939);
#2892=LINE('',#15819,#3940);
#2893=LINE('',#15820,#3941);
#2894=LINE('',#15822,#3942);
#2895=LINE('',#15824,#3943);
#2896=LINE('',#15828,#3944);
#2897=LINE('',#15830,#3945);
#2898=LINE('',#15831,#3946);
#2899=LINE('',#15834,#3947);
#2900=LINE('',#15836,#3948);
#2901=LINE('',#15837,#3949);
#2902=LINE('',#15839,#3950);
#2903=LINE('',#15841,#3951);
#2904=LINE('',#15845,#3952);
#2905=LINE('',#15847,#3953);
#2906=LINE('',#15848,#3954);
#2907=LINE('',#15851,#3955);
#2908=LINE('',#15853,#3956);
#2909=LINE('',#15854,#3957);
#2910=LINE('',#15856,#3958);
#2911=LINE('',#15858,#3959);
#2912=LINE('',#15862,#3960);
#2913=LINE('',#15864,#3961);
#2914=LINE('',#15865,#3962);
#2915=LINE('',#15868,#3963);
#2916=LINE('',#15870,#3964);
#2917=LINE('',#15871,#3965);
#2918=LINE('',#15873,#3966);
#2919=LINE('',#15875,#3967);
#2920=LINE('',#15879,#3968);
#2921=LINE('',#15881,#3969);
#2922=LINE('',#15882,#3970);
#2923=LINE('',#15885,#3971);
#2924=LINE('',#15887,#3972);
#2925=LINE('',#15888,#3973);
#2926=LINE('',#15890,#3974);
#2927=LINE('',#15892,#3975);
#2928=LINE('',#15896,#3976);
#2929=LINE('',#15898,#3977);
#2930=LINE('',#15899,#3978);
#2931=LINE('',#15902,#3979);
#2932=LINE('',#15904,#3980);
#2933=LINE('',#15905,#3981);
#2934=LINE('',#15907,#3982);
#2935=LINE('',#15909,#3983);
#2936=LINE('',#15913,#3984);
#2937=LINE('',#15915,#3985);
#2938=LINE('',#15916,#3986);
#2939=LINE('',#15919,#3987);
#2940=LINE('',#15921,#3988);
#2941=LINE('',#15922,#3989);
#2942=LINE('',#15924,#3990);
#2943=LINE('',#15926,#3991);
#2944=LINE('',#15930,#3992);
#2945=LINE('',#15932,#3993);
#2946=LINE('',#15933,#3994);
#2947=LINE('',#15936,#3995);
#2948=LINE('',#15938,#3996);
#2949=LINE('',#15939,#3997);
#2950=LINE('',#15941,#3998);
#2951=LINE('',#15943,#3999);
#2952=LINE('',#15947,#4000);
#2953=LINE('',#15949,#4001);
#2954=LINE('',#15950,#4002);
#2955=LINE('',#15953,#4003);
#2956=LINE('',#15955,#4004);
#2957=LINE('',#15956,#4005);
#2958=LINE('',#15958,#4006);
#2959=LINE('',#15960,#4007);
#2960=LINE('',#15964,#4008);
#2961=LINE('',#15966,#4009);
#2962=LINE('',#15967,#4010);
#2963=LINE('',#15970,#4011);
#2964=LINE('',#15972,#4012);
#2965=LINE('',#15973,#4013);
#2966=LINE('',#15975,#4014);
#2967=LINE('',#15977,#4015);
#2968=LINE('',#15981,#4016);
#2969=LINE('',#15983,#4017);
#2970=LINE('',#15984,#4018);
#2971=LINE('',#15987,#4019);
#2972=LINE('',#15989,#4020);
#2973=LINE('',#15990,#4021);
#2974=LINE('',#15992,#4022);
#2975=LINE('',#15994,#4023);
#2976=LINE('',#15998,#4024);
#2977=LINE('',#16000,#4025);
#2978=LINE('',#16001,#4026);
#2979=LINE('',#16004,#4027);
#2980=LINE('',#16006,#4028);
#2981=LINE('',#16007,#4029);
#2982=LINE('',#16009,#4030);
#2983=LINE('',#16011,#4031);
#2984=LINE('',#16015,#4032);
#2985=LINE('',#16017,#4033);
#2986=LINE('',#16018,#4034);
#2987=LINE('',#16021,#4035);
#2988=LINE('',#16023,#4036);
#2989=LINE('',#16024,#4037);
#2990=LINE('',#16026,#4038);
#2991=LINE('',#16028,#4039);
#2992=LINE('',#16032,#4040);
#2993=LINE('',#16034,#4041);
#2994=LINE('',#16035,#4042);
#2995=LINE('',#16038,#4043);
#2996=LINE('',#16040,#4044);
#2997=LINE('',#16041,#4045);
#2998=LINE('',#16043,#4046);
#2999=LINE('',#16045,#4047);
#3000=LINE('',#16049,#4048);
#3001=LINE('',#16051,#4049);
#3002=LINE('',#16052,#4050);
#3003=LINE('',#16055,#4051);
#3004=LINE('',#16057,#4052);
#3005=LINE('',#16058,#4053);
#3006=LINE('',#16060,#4054);
#3007=LINE('',#16062,#4055);
#3008=LINE('',#16066,#4056);
#3009=LINE('',#16068,#4057);
#3010=LINE('',#16069,#4058);
#3011=LINE('',#16072,#4059);
#3012=LINE('',#16074,#4060);
#3013=LINE('',#16075,#4061);
#3014=LINE('',#16077,#4062);
#3015=LINE('',#16079,#4063);
#3016=LINE('',#16083,#4064);
#3017=LINE('',#16085,#4065);
#3018=LINE('',#16086,#4066);
#3019=LINE('',#16089,#4067);
#3020=LINE('',#16091,#4068);
#3021=LINE('',#16092,#4069);
#3022=LINE('',#16094,#4070);
#3023=LINE('',#16096,#4071);
#3024=LINE('',#16100,#4072);
#3025=LINE('',#16102,#4073);
#3026=LINE('',#16103,#4074);
#3027=LINE('',#16106,#4075);
#3028=LINE('',#16108,#4076);
#3029=LINE('',#16109,#4077);
#3030=LINE('',#16111,#4078);
#3031=LINE('',#16113,#4079);
#3032=LINE('',#16117,#4080);
#3033=LINE('',#16119,#4081);
#3034=LINE('',#16120,#4082);
#3035=LINE('',#16123,#4083);
#3036=LINE('',#16125,#4084);
#3037=LINE('',#16126,#4085);
#3038=LINE('',#16128,#4086);
#3039=LINE('',#16130,#4087);
#3040=LINE('',#16134,#4088);
#3041=LINE('',#16136,#4089);
#3042=LINE('',#16137,#4090);
#3043=LINE('',#16140,#4091);
#3044=LINE('',#16142,#4092);
#3045=LINE('',#16143,#4093);
#3046=LINE('',#16145,#4094);
#3047=LINE('',#16147,#4095);
#3048=LINE('',#16151,#4096);
#3049=LINE('',#16153,#4097);
#3050=LINE('',#16154,#4098);
#3051=LINE('',#16157,#4099);
#3052=LINE('',#16159,#4100);
#3053=LINE('',#16160,#4101);
#3054=LINE('',#16162,#4102);
#3055=LINE('',#16164,#4103);
#3056=LINE('',#16171,#4104);
#3057=LINE('',#16177,#4105);
#3058=LINE('',#16182,#4106);
#3059=LINE('',#16184,#4107);
#3060=LINE('',#16186,#4108);
#3061=LINE('',#16188,#4109);
#3062=LINE('',#16190,#4110);
#3063=LINE('',#16192,#4111);
#3064=LINE('',#16194,#4112);
#3065=LINE('',#16196,#4113);
#3066=LINE('',#16198,#4114);
#3067=LINE('',#16200,#4115);
#3068=LINE('',#16202,#4116);
#3069=LINE('',#16204,#4117);
#3070=LINE('',#16206,#4118);
#3071=LINE('',#16207,#4119);
#3072=LINE('',#16211,#4120);
#3073=LINE('',#16213,#4121);
#3074=LINE('',#16215,#4122);
#3075=LINE('',#16217,#4123);
#3076=LINE('',#16219,#4124);
#3077=LINE('',#16221,#4125);
#3078=LINE('',#16223,#4126);
#3079=LINE('',#16225,#4127);
#3080=LINE('',#16227,#4128);
#3081=LINE('',#16229,#4129);
#3082=LINE('',#16231,#4130);
#3083=LINE('',#16233,#4131);
#3084=LINE('',#16235,#4132);
#3085=LINE('',#16236,#4133);
#3086=LINE('',#16238,#4134);
#3087=LINE('',#16239,#4135);
#3088=LINE('',#16241,#4136);
#3089=LINE('',#16243,#4137);
#3090=LINE('',#16245,#4138);
#3091=LINE('',#16247,#4139);
#3092=LINE('',#16249,#4140);
#3093=LINE('',#16251,#4141);
#3094=LINE('',#16253,#4142);
#3095=LINE('',#16255,#4143);
#3096=LINE('',#16257,#4144);
#3097=LINE('',#16259,#4145);
#3098=LINE('',#16261,#4146);
#3099=LINE('',#16263,#4147);
#3100=LINE('',#16270,#4148);
#3101=LINE('',#16277,#4149);
#3102=LINE('',#16280,#4150);
#3103=LINE('',#16286,#4151);
#3104=LINE('',#16295,#4152);
#3105=LINE('',#16301,#4153);
#3106=LINE('',#16311,#4154);
#3107=LINE('',#16316,#4155);
#3108=LINE('',#16318,#4156);
#3109=LINE('',#16320,#4157);
#3110=LINE('',#16322,#4158);
#3111=LINE('',#16324,#4159);
#3112=LINE('',#16325,#4160);
#3113=LINE('',#16329,#4161);
#3114=LINE('',#16331,#4162);
#3115=LINE('',#16333,#4163);
#3116=LINE('',#16335,#4164);
#3117=LINE('',#16337,#4165);
#3118=LINE('',#16338,#4166);
#3119=LINE('',#16340,#4167);
#3120=LINE('',#16341,#4168);
#3121=LINE('',#16343,#4169);
#3122=LINE('',#16345,#4170);
#3123=LINE('',#16347,#4171);
#3124=LINE('',#16349,#4172);
#3125=LINE('',#16356,#4173);
#3126=LINE('',#16362,#4174);
#3127=LINE('',#16367,#4175);
#3128=LINE('',#16369,#4176);
#3129=LINE('',#16371,#4177);
#3130=LINE('',#16373,#4178);
#3131=LINE('',#16375,#4179);
#3132=LINE('',#16376,#4180);
#3133=LINE('',#16381,#4181);
#3134=LINE('',#16383,#4182);
#3135=LINE('',#16384,#4183);
#3136=LINE('',#16387,#4184);
#3137=LINE('',#16388,#4185);
#3138=LINE('',#16391,#4186);
#3139=LINE('',#16392,#4187);
#3140=LINE('',#16395,#4188);
#3141=LINE('',#16396,#4189);
#3142=LINE('',#16399,#4190);
#3143=LINE('',#16400,#4191);
#3144=LINE('',#16402,#4192);
#3145=LINE('',#16409,#4193);
#3146=LINE('',#16414,#4194);
#3147=LINE('',#16416,#4195);
#3148=LINE('',#16418,#4196);
#3149=LINE('',#16419,#4197);
#3150=LINE('',#16422,#4198);
#3151=LINE('',#16424,#4199);
#3152=LINE('',#16425,#4200);
#3153=LINE('',#16428,#4201);
#3154=LINE('',#16430,#4202);
#3155=LINE('',#16431,#4203);
#3156=LINE('',#16434,#4204);
#3157=LINE('',#16436,#4205);
#3158=LINE('',#16437,#4206);
#3159=LINE('',#16440,#4207);
#3160=LINE('',#16442,#4208);
#3161=LINE('',#16443,#4209);
#3162=LINE('',#16445,#4210);
#3163=LINE('',#16446,#4211);
#3164=LINE('',#16455,#4212);
#3165=LINE('',#16461,#4213);
#3166=LINE('',#16466,#4214);
#3167=LINE('',#16468,#4215);
#3168=LINE('',#16470,#4216);
#3169=LINE('',#16472,#4217);
#3170=LINE('',#16474,#4218);
#3171=LINE('',#16475,#4219);
#3172=LINE('',#16480,#4220);
#3173=LINE('',#16482,#4221);
#3174=LINE('',#16483,#4222);
#3175=LINE('',#16486,#4223);
#3176=LINE('',#16487,#4224);
#3177=LINE('',#16490,#4225);
#3178=LINE('',#16491,#4226);
#3179=LINE('',#16494,#4227);
#3180=LINE('',#16495,#4228);
#3181=LINE('',#16498,#4229);
#3182=LINE('',#16499,#4230);
#3183=LINE('',#16501,#4231);
#3184=VECTOR('',#10936,2.5);
#3185=VECTOR('',#10943,2.5);
#3186=VECTOR('',#10948,1000.);
#3187=VECTOR('',#10949,1000.);
#3188=VECTOR('',#10950,1000.);
#3189=VECTOR('',#10951,1000.);
#3190=VECTOR('',#10952,1000.);
#3191=VECTOR('',#10953,1000.);
#3192=VECTOR('',#10954,1000.);
#3193=VECTOR('',#10955,1000.);
#3194=VECTOR('',#10956,1000.);
#3195=VECTOR('',#10957,1000.);
#3196=VECTOR('',#10958,1000.);
#3197=VECTOR('',#10959,1000.);
#3198=VECTOR('',#10960,1000.);
#3199=VECTOR('',#10961,1000.);
#3200=VECTOR('',#10962,1000.);
#3201=VECTOR('',#10963,1000.);
#3202=VECTOR('',#10964,1000.);
#3203=VECTOR('',#10965,1000.);
#3204=VECTOR('',#10966,1000.);
#3205=VECTOR('',#10967,1000.);
#3206=VECTOR('',#10968,1000.);
#3207=VECTOR('',#10969,1000.);
#3208=VECTOR('',#10970,1000.);
#3209=VECTOR('',#10971,1000.);
#3210=VECTOR('',#10972,1000.);
#3211=VECTOR('',#10973,1000.);
#3212=VECTOR('',#10974,1000.);
#3213=VECTOR('',#10975,1000.);
#3214=VECTOR('',#10976,1000.);
#3215=VECTOR('',#10977,1000.);
#3216=VECTOR('',#10978,1000.);
#3217=VECTOR('',#10979,1000.);
#3218=VECTOR('',#10980,1000.);
#3219=VECTOR('',#10981,1000.);
#3220=VECTOR('',#10982,1000.);
#3221=VECTOR('',#10983,1000.);
#3222=VECTOR('',#10984,1000.);
#3223=VECTOR('',#10985,1000.);
#3224=VECTOR('',#10986,1000.);
#3225=VECTOR('',#10987,1000.);
#3226=VECTOR('',#10990,1000.);
#3227=VECTOR('',#10991,1000.);
#3228=VECTOR('',#10992,1000.);
#3229=VECTOR('',#10995,1000.);
#3230=VECTOR('',#10996,1000.);
#3231=VECTOR('',#10997,1000.);
#3232=VECTOR('',#11000,1000.);
#3233=VECTOR('',#11001,1000.);
#3234=VECTOR('',#11002,1000.);
#3235=VECTOR('',#11005,1000.);
#3236=VECTOR('',#11006,1000.);
#3237=VECTOR('',#11007,1000.);
#3238=VECTOR('',#11010,1000.);
#3239=VECTOR('',#11011,1000.);
#3240=VECTOR('',#11012,1000.);
#3241=VECTOR('',#11015,1000.);
#3242=VECTOR('',#11016,1000.);
#3243=VECTOR('',#11017,1000.);
#3244=VECTOR('',#11020,1000.);
#3245=VECTOR('',#11021,1000.);
#3246=VECTOR('',#11022,1000.);
#3247=VECTOR('',#11025,1000.);
#3248=VECTOR('',#11026,1000.);
#3249=VECTOR('',#11027,1000.);
#3250=VECTOR('',#11030,1000.);
#3251=VECTOR('',#11031,1000.);
#3252=VECTOR('',#11032,1000.);
#3253=VECTOR('',#11033,1000.);
#3254=VECTOR('',#11034,1000.);
#3255=VECTOR('',#11035,1000.);
#3256=VECTOR('',#11036,1000.);
#3257=VECTOR('',#11037,1000.);
#3258=VECTOR('',#11038,1000.);
#3259=VECTOR('',#11039,1000.);
#3260=VECTOR('',#11040,1000.);
#3261=VECTOR('',#11041,1000.);
#3262=VECTOR('',#11042,1000.);
#3263=VECTOR('',#11043,1000.);
#3264=VECTOR('',#11044,1000.);
#3265=VECTOR('',#11045,1000.);
#3266=VECTOR('',#11046,1000.);
#3267=VECTOR('',#11047,1000.);
#3268=VECTOR('',#11048,1000.);
#3269=VECTOR('',#11049,1000.);
#3270=VECTOR('',#11058,1000.);
#3271=VECTOR('',#11059,1000.);
#3272=VECTOR('',#11060,1000.);
#3273=VECTOR('',#11063,1000.);
#3274=VECTOR('',#11064,1000.);
#3275=VECTOR('',#11065,1000.);
#3276=VECTOR('',#11068,1000.);
#3277=VECTOR('',#11069,1000.);
#3278=VECTOR('',#11070,1000.);
#3279=VECTOR('',#11073,1000.);
#3280=VECTOR('',#11074,1000.);
#3281=VECTOR('',#11081,1000.);
#3282=VECTOR('',#11082,1000.);
#3283=VECTOR('',#11083,1000.);
#3284=VECTOR('',#11086,1000.);
#3285=VECTOR('',#11087,1000.);
#3286=VECTOR('',#11088,1000.);
#3287=VECTOR('',#11091,1000.);
#3288=VECTOR('',#11092,1000.);
#3289=VECTOR('',#11093,1000.);
#3290=VECTOR('',#11096,1000.);
#3291=VECTOR('',#11097,1000.);
#3292=VECTOR('',#11104,1000.);
#3293=VECTOR('',#11107,1000.);
#3294=VECTOR('',#11112,1000.);
#3295=VECTOR('',#11115,1000.);
#3296=VECTOR('',#11120,1000.);
#3297=VECTOR('',#11123,1000.);
#3298=VECTOR('',#11128,1000.);
#3299=VECTOR('',#11131,1000.);
#3300=VECTOR('',#11136,1000.);
#3301=VECTOR('',#11139,1000.);
#3302=VECTOR('',#11144,1000.);
#3303=VECTOR('',#11147,1000.);
#3304=VECTOR('',#11166,1000.);
#3305=VECTOR('',#11169,1000.);
#3306=VECTOR('',#11174,2.5);
#3307=VECTOR('',#11181,2.5);
#3308=VECTOR('',#11188,2.6);
#3309=VECTOR('',#11199,2.6);
#3310=VECTOR('',#11210,2.6);
#3311=VECTOR('',#11219,1000.);
#3312=VECTOR('',#11220,1000.);
#3313=VECTOR('',#11221,1000.);
#3314=VECTOR('',#11222,1000.);
#3315=VECTOR('',#11223,1000.);
#3316=VECTOR('',#11224,1000.);
#3317=VECTOR('',#11225,1000.);
#3318=VECTOR('',#11226,1000.);
#3319=VECTOR('',#11227,1000.);
#3320=VECTOR('',#11228,1000.);
#3321=VECTOR('',#11229,1000.);
#3322=VECTOR('',#11230,1000.);
#3323=VECTOR('',#11231,1000.);
#3324=VECTOR('',#11232,1000.);
#3325=VECTOR('',#11235,1000.);
#3326=VECTOR('',#11236,1000.);
#3327=VECTOR('',#11237,1000.);
#3328=VECTOR('',#11238,1000.);
#3329=VECTOR('',#11239,1000.);
#3330=VECTOR('',#11240,1000.);
#3331=VECTOR('',#11241,1000.);
#3332=VECTOR('',#11244,1000.);
#3333=VECTOR('',#11245,1000.);
#3334=VECTOR('',#11246,1000.);
#3335=VECTOR('',#11249,1000.);
#3336=VECTOR('',#11250,1000.);
#3337=VECTOR('',#11251,1000.);
#3338=VECTOR('',#11254,1000.);
#3339=VECTOR('',#11255,1000.);
#3340=VECTOR('',#11256,1000.);
#3341=VECTOR('',#11259,1000.);
#3342=VECTOR('',#11260,1000.);
#3343=VECTOR('',#11261,1000.);
#3344=VECTOR('',#11264,1000.);
#3345=VECTOR('',#11265,1000.);
#3346=VECTOR('',#11266,1000.);
#3347=VECTOR('',#11269,1000.);
#3348=VECTOR('',#11270,1000.);
#3349=VECTOR('',#11273,1000.);
#3350=VECTOR('',#11274,1000.);
#3351=VECTOR('',#11275,1000.);
#3352=VECTOR('',#11278,1000.);
#3353=VECTOR('',#11279,1000.);
#3354=VECTOR('',#11280,1000.);
#3355=VECTOR('',#11283,1000.);
#3356=VECTOR('',#11284,1000.);
#3357=VECTOR('',#11285,1000.);
#3358=VECTOR('',#11288,1000.);
#3359=VECTOR('',#11289,1000.);
#3360=VECTOR('',#11296,1000.);
#3361=VECTOR('',#11297,1000.);
#3362=VECTOR('',#11298,1000.);
#3363=VECTOR('',#11301,1000.);
#3364=VECTOR('',#11302,1000.);
#3365=VECTOR('',#11303,1000.);
#3366=VECTOR('',#11306,1000.);
#3367=VECTOR('',#11307,1000.);
#3368=VECTOR('',#11308,1000.);
#3369=VECTOR('',#11311,1000.);
#3370=VECTOR('',#11312,1000.);
#3371=VECTOR('',#11319,1000.);
#3372=VECTOR('',#11320,1000.);
#3373=VECTOR('',#11321,1000.);
#3374=VECTOR('',#11324,1000.);
#3375=VECTOR('',#11325,1000.);
#3376=VECTOR('',#11326,1000.);
#3377=VECTOR('',#11329,1000.);
#3378=VECTOR('',#11330,1000.);
#3379=VECTOR('',#11331,1000.);
#3380=VECTOR('',#11334,1000.);
#3381=VECTOR('',#11335,1000.);
#3382=VECTOR('',#11358,2.59999999999999);
#3383=VECTOR('',#11369,2.59999999999999);
#3384=VECTOR('',#11380,2.59999999999999);
#3385=VECTOR('',#11391,2.5);
#3386=VECTOR('',#11398,2.5);
#3387=VECTOR('',#11405,9.1);
#3388=VECTOR('',#11410,1000.);
#3389=VECTOR('',#11411,1000.);
#3390=VECTOR('',#11412,1000.);
#3391=VECTOR('',#11413,1000.);
#3392=VECTOR('',#11414,1000.);
#3393=VECTOR('',#11415,1000.);
#3394=VECTOR('',#11416,1000.);
#3395=VECTOR('',#11417,1000.);
#3396=VECTOR('',#11418,1000.);
#3397=VECTOR('',#11419,1000.);
#3398=VECTOR('',#11420,1000.);
#3399=VECTOR('',#11421,1000.);
#3400=VECTOR('',#11422,1000.);
#3401=VECTOR('',#11423,1000.);
#3402=VECTOR('',#11424,1000.);
#3403=VECTOR('',#11425,1000.);
#3404=VECTOR('',#11426,1000.);
#3405=VECTOR('',#11427,1000.);
#3406=VECTOR('',#11428,1000.);
#3407=VECTOR('',#11429,1000.);
#3408=VECTOR('',#11430,1000.);
#3409=VECTOR('',#11431,1000.);
#3410=VECTOR('',#11432,1000.);
#3411=VECTOR('',#11433,1000.);
#3412=VECTOR('',#11436,1000.);
#3413=VECTOR('',#11437,1000.);
#3414=VECTOR('',#11438,1000.);
#3415=VECTOR('',#11439,1000.);
#3416=VECTOR('',#11440,1000.);
#3417=VECTOR('',#11441,1000.);
#3418=VECTOR('',#11442,1000.);
#3419=VECTOR('',#11443,1000.);
#3420=VECTOR('',#11444,1000.);
#3421=VECTOR('',#11445,1000.);
#3422=VECTOR('',#11446,1000.);
#3423=VECTOR('',#11447,1000.);
#3424=VECTOR('',#11450,1000.);
#3425=VECTOR('',#11451,1000.);
#3426=VECTOR('',#11452,1000.);
#3427=VECTOR('',#11453,1000.);
#3428=VECTOR('',#11454,1000.);
#3429=VECTOR('',#11455,1000.);
#3430=VECTOR('',#11458,1000.);
#3431=VECTOR('',#11459,1000.);
#3432=VECTOR('',#11460,1000.);
#3433=VECTOR('',#11463,1000.);
#3434=VECTOR('',#11464,1000.);
#3435=VECTOR('',#11465,1000.);
#3436=VECTOR('',#11468,1000.);
#3437=VECTOR('',#11469,1000.);
#3438=VECTOR('',#11470,1000.);
#3439=VECTOR('',#11473,1000.);
#3440=VECTOR('',#11474,1000.);
#3441=VECTOR('',#11475,1000.);
#3442=VECTOR('',#11478,1000.);
#3443=VECTOR('',#11479,1000.);
#3444=VECTOR('',#11480,1000.);
#3445=VECTOR('',#11483,1000.);
#3446=VECTOR('',#11484,1000.);
#3447=VECTOR('',#11485,1000.);
#3448=VECTOR('',#11488,1000.);
#3449=VECTOR('',#11489,1000.);
#3450=VECTOR('',#11490,1000.);
#3451=VECTOR('',#11491,1000.);
#3452=VECTOR('',#11494,1000.);
#3453=VECTOR('',#11495,1000.);
#3454=VECTOR('',#11496,1000.);
#3455=VECTOR('',#11497,1000.);
#3456=VECTOR('',#11500,1000.);
#3457=VECTOR('',#11501,1000.);
#3458=VECTOR('',#11502,1000.);
#3459=VECTOR('',#11505,1000.);
#3460=VECTOR('',#11506,1000.);
#3461=VECTOR('',#11507,1000.);
#3462=VECTOR('',#11510,1000.);
#3463=VECTOR('',#11511,1000.);
#3464=VECTOR('',#11512,1000.);
#3465=VECTOR('',#11513,1000.);
#3466=VECTOR('',#11514,1000.);
#3467=VECTOR('',#11515,1000.);
#3468=VECTOR('',#11518,1000.);
#3469=VECTOR('',#11519,1000.);
#3470=VECTOR('',#11520,1000.);
#3471=VECTOR('',#11521,1000.);
#3472=VECTOR('',#11522,1000.);
#3473=VECTOR('',#11525,1000.);
#3474=VECTOR('',#11528,1000.);
#3475=VECTOR('',#11529,1000.);
#3476=VECTOR('',#11532,1000.);
#3477=VECTOR('',#11533,1000.);
#3478=VECTOR('',#11536,1000.);
#3479=VECTOR('',#11537,1000.);
#3480=VECTOR('',#11540,1000.);
#3481=VECTOR('',#11541,1000.);
#3482=VECTOR('',#11542,1000.);
#3483=VECTOR('',#11543,1000.);
#3484=VECTOR('',#11546,1000.);
#3485=VECTOR('',#11549,1000.);
#3486=VECTOR('',#11550,1000.);
#3487=VECTOR('',#11551,1000.);
#3488=VECTOR('',#11552,1000.);
#3489=VECTOR('',#11553,1000.);
#3490=VECTOR('',#11556,1000.);
#3491=VECTOR('',#11559,1000.);
#3492=VECTOR('',#11560,1000.);
#3493=VECTOR('',#11561,1000.);
#3494=VECTOR('',#11562,1000.);
#3495=VECTOR('',#11563,1000.);
#3496=VECTOR('',#11566,1000.);
#3497=VECTOR('',#11567,1000.);
#3498=VECTOR('',#11570,1000.);
#3499=VECTOR('',#11571,1000.);
#3500=VECTOR('',#11574,1000.);
#3501=VECTOR('',#11575,1000.);
#3502=VECTOR('',#11578,1000.);
#3503=VECTOR('',#11579,1000.);
#3504=VECTOR('',#11582,1000.);
#3505=VECTOR('',#11587,1000.);
#3506=VECTOR('',#11588,1000.);
#3507=VECTOR('',#11591,1000.);
#3508=VECTOR('',#11592,1000.);
#3509=VECTOR('',#11595,1000.);
#3510=VECTOR('',#11596,1000.);
#3511=VECTOR('',#11599,1000.);
#3512=VECTOR('',#11600,1000.);
#3513=VECTOR('',#11603,1000.);
#3514=VECTOR('',#11608,1000.);
#3515=VECTOR('',#11609,1000.);
#3516=VECTOR('',#11612,1000.);
#3517=VECTOR('',#11613,1000.);
#3518=VECTOR('',#11616,1000.);
#3519=VECTOR('',#11617,1000.);
#3520=VECTOR('',#11618,1000.);
#3521=VECTOR('',#11619,1000.);
#3522=VECTOR('',#11620,1000.);
#3523=VECTOR('',#11623,1000.);
#3524=VECTOR('',#11624,1000.);
#3525=VECTOR('',#11625,1000.);
#3526=VECTOR('',#11626,1000.);
#3527=VECTOR('',#11627,1000.);
#3528=VECTOR('',#11644,1000.);
#3529=VECTOR('',#11659,1.65);
#3530=VECTOR('',#11666,1.65);
#3531=VECTOR('',#11673,2.5);
#3532=VECTOR('',#11680,2.5);
#3533=VECTOR('',#11687,6.15);
#3534=VECTOR('',#11692,1000.);
#3535=VECTOR('',#11693,1000.);
#3536=VECTOR('',#11694,1000.);
#3537=VECTOR('',#11695,1000.);
#3538=VECTOR('',#11698,1000.);
#3539=VECTOR('',#11699,1000.);
#3540=VECTOR('',#11700,1000.);
#3541=VECTOR('',#11701,1000.);
#3542=VECTOR('',#11704,1000.);
#3543=VECTOR('',#11705,1000.);
#3544=VECTOR('',#11706,1000.);
#3545=VECTOR('',#11709,1000.);
#3546=VECTOR('',#11710,1000.);
#3547=VECTOR('',#11711,1000.);
#3548=VECTOR('',#11714,1000.);
#3549=VECTOR('',#11715,1000.);
#3550=VECTOR('',#11716,1000.);
#3551=VECTOR('',#11719,1000.);
#3552=VECTOR('',#11720,1000.);
#3553=VECTOR('',#11721,1000.);
#3554=VECTOR('',#11724,1000.);
#3555=VECTOR('',#11725,1000.);
#3556=VECTOR('',#11728,1000.);
#3557=VECTOR('',#11729,1000.);
#3558=VECTOR('',#11730,1000.);
#3559=VECTOR('',#11733,1000.);
#3560=VECTOR('',#11734,1000.);
#3561=VECTOR('',#11735,1000.);
#3562=VECTOR('',#11738,1000.);
#3563=VECTOR('',#11741,1000.);
#3564=VECTOR('',#11758,1000.);
#3565=VECTOR('',#11759,1000.);
#3566=VECTOR('',#11760,1000.);
#3567=VECTOR('',#11761,1000.);
#3568=VECTOR('',#11764,1000.);
#3569=VECTOR('',#11765,1000.);
#3570=VECTOR('',#11766,1000.);
#3571=VECTOR('',#11769,1000.);
#3572=VECTOR('',#11770,1000.);
#3573=VECTOR('',#11771,1000.);
#3574=VECTOR('',#11774,1000.);
#3575=VECTOR('',#11775,1000.);
#3576=VECTOR('',#11784,1000.);
#3577=VECTOR('',#11785,1000.);
#3578=VECTOR('',#11786,1000.);
#3579=VECTOR('',#11787,1000.);
#3580=VECTOR('',#11790,1000.);
#3581=VECTOR('',#11791,1000.);
#3582=VECTOR('',#11792,1000.);
#3583=VECTOR('',#11795,1000.);
#3584=VECTOR('',#11796,1000.);
#3585=VECTOR('',#11797,1000.);
#3586=VECTOR('',#11800,1000.);
#3587=VECTOR('',#11801,1000.);
#3588=VECTOR('',#11812,3.7);
#3589=VECTOR('',#11819,3.7);
#3590=VECTOR('',#11826,2.2);
#3591=VECTOR('',#11833,2.2);
#3592=VECTOR('',#11838,1000.);
#3593=VECTOR('',#11839,1000.);
#3594=VECTOR('',#11840,1000.);
#3595=VECTOR('',#11841,1000.);
#3596=VECTOR('',#11844,1000.);
#3597=VECTOR('',#11845,1000.);
#3598=VECTOR('',#11846,1000.);
#3599=VECTOR('',#11849,1000.);
#3600=VECTOR('',#11850,1000.);
#3601=VECTOR('',#11851,1000.);
#3602=VECTOR('',#11854,1000.);
#3603=VECTOR('',#11855,1000.);
#3604=VECTOR('',#11870,5.55);
#3605=VECTOR('',#11877,6.);
#3606=VECTOR('',#11884,9.);
#3607=VECTOR('',#11891,6.);
#3608=VECTOR('',#11898,4.);
#3609=VECTOR('',#11919,7.15);
#3610=VECTOR('',#11926,6.);
#3611=VECTOR('',#11933,9.);
#3612=VECTOR('',#11940,6.);
#3613=VECTOR('',#11947,4.);
#3614=VECTOR('',#11968,2.2);
#3615=VECTOR('',#11971,2.2);
#3616=VECTOR('',#11978,6.);
#3617=VECTOR('',#11985,8.75);
#3618=VECTOR('',#11992,1000.);
#3619=VECTOR('',#11995,1000.);
#3620=VECTOR('',#11998,10.);
#3621=VECTOR('',#11999,10.);
#3622=VECTOR('',#12004,1000.);
#3623=VECTOR('',#12007,1000.);
#3624=VECTOR('',#12010,1000.);
#3625=VECTOR('',#12013,1000.);
#3626=VECTOR('',#12022,1000.);
#3627=VECTOR('',#12025,1000.);
#3628=VECTOR('',#12034,5.75);
#3629=VECTOR('',#12039,1000.);
#3630=VECTOR('',#12040,1000.);
#3631=VECTOR('',#12041,1000.);
#3632=VECTOR('',#12042,1000.);
#3633=VECTOR('',#12045,1000.);
#3634=VECTOR('',#12046,1000.);
#3635=VECTOR('',#12047,1000.);
#3636=VECTOR('',#12048,1000.);
#3637=VECTOR('',#12051,1000.);
#3638=VECTOR('',#12052,1000.);
#3639=VECTOR('',#12055,1000.);
#3640=VECTOR('',#12058,1000.);
#3641=VECTOR('',#12067,7.35);
#3642=VECTOR('',#12072,1000.);
#3643=VECTOR('',#12073,1000.);
#3644=VECTOR('',#12074,1000.);
#3645=VECTOR('',#12075,1000.);
#3646=VECTOR('',#12078,1000.);
#3647=VECTOR('',#12079,1000.);
#3648=VECTOR('',#12080,1000.);
#3649=VECTOR('',#12081,1000.);
#3650=VECTOR('',#12084,1000.);
#3651=VECTOR('',#12085,1000.);
#3652=VECTOR('',#12088,1000.);
#3653=VECTOR('',#12091,1000.);
#3654=VECTOR('',#12100,2.19999999999999);
#3655=VECTOR('',#12113,5.);
#3656=VECTOR('',#12120,3.);
#3657=VECTOR('',#12135,2.);
#3658=VECTOR('',#12148,5.50000000000001);
#3659=VECTOR('',#12155,5.50000000000001);
#3660=VECTOR('',#12162,3.3);
#3661=VECTOR('',#12169,3.3);
#3662=VECTOR('',#12174,1000.);
#3663=VECTOR('',#12175,1000.);
#3664=VECTOR('',#12176,1000.);
#3665=VECTOR('',#12177,1000.);
#3666=VECTOR('',#12180,1000.);
#3667=VECTOR('',#12181,1000.);
#3668=VECTOR('',#12182,1000.);
#3669=VECTOR('',#12185,1000.);
#3670=VECTOR('',#12186,1000.);
#3671=VECTOR('',#12187,1000.);
#3672=VECTOR('',#12190,1000.);
#3673=VECTOR('',#12191,1000.);
#3674=VECTOR('',#12206,3.3);
#3675=VECTOR('',#12213,3.3);
#3676=VECTOR('',#12220,6.2);
#3677=VECTOR('',#12225,1000.);
#3678=VECTOR('',#12226,1000.);
#3679=VECTOR('',#12227,1000.);
#3680=VECTOR('',#12228,1000.);
#3681=VECTOR('',#12229,1000.);
#3682=VECTOR('',#12230,1000.);
#3683=VECTOR('',#12231,1000.);
#3684=VECTOR('',#12232,1000.);
#3685=VECTOR('',#12235,1000.);
#3686=VECTOR('',#12236,1000.);
#3687=VECTOR('',#12237,1000.);
#3688=VECTOR('',#12238,1000.);
#3689=VECTOR('',#12239,1000.);
#3690=VECTOR('',#12240,1000.);
#3691=VECTOR('',#12241,1000.);
#3692=VECTOR('',#12242,1000.);
#3693=VECTOR('',#12245,1000.);
#3694=VECTOR('',#12246,1000.);
#3695=VECTOR('',#12249,1000.);
#3696=VECTOR('',#12252,1000.);
#3697=VECTOR('',#12255,1000.);
#3698=VECTOR('',#12258,1000.);
#3699=VECTOR('',#12261,1000.);
#3700=VECTOR('',#12264,1000.);
#3701=VECTOR('',#12273,6.2);
#3702=VECTOR('',#12280,14.);
#3703=VECTOR('',#12283,1000.);
#3704=VECTOR('',#12286,14.);
#3705=VECTOR('',#12291,1000.);
#3706=VECTOR('',#12296,1000.);
#3707=VECTOR('',#12299,1000.);
#3708=VECTOR('',#12300,1000.);
#3709=VECTOR('',#12303,1000.);
#3710=VECTOR('',#12306,1000.);
#3711=VECTOR('',#12309,1000.);
#3712=VECTOR('',#12312,1000.);
#3713=VECTOR('',#12315,1000.);
#3714=VECTOR('',#12318,1000.);
#3715=VECTOR('',#12321,1000.);
#3716=VECTOR('',#12324,1000.);
#3717=VECTOR('',#12327,1000.);
#3718=VECTOR('',#12330,1000.);
#3719=VECTOR('',#12333,1000.);
#3720=VECTOR('',#12336,1000.);
#3721=VECTOR('',#12339,1000.);
#3722=VECTOR('',#12342,1000.);
#3723=VECTOR('',#12345,1000.);
#3724=VECTOR('',#12348,1000.);
#3725=VECTOR('',#12351,1000.);
#3726=VECTOR('',#12354,1000.);
#3727=VECTOR('',#12357,1000.);
#3728=VECTOR('',#12360,1000.);
#3729=VECTOR('',#12363,1000.);
#3730=VECTOR('',#12366,1000.);
#3731=VECTOR('',#12369,1000.);
#3732=VECTOR('',#12372,1000.);
#3733=VECTOR('',#12375,1000.);
#3734=VECTOR('',#12378,1000.);
#3735=VECTOR('',#12381,1000.);
#3736=VECTOR('',#12384,1000.);
#3737=VECTOR('',#12387,1000.);
#3738=VECTOR('',#12390,1000.);
#3739=VECTOR('',#12393,1000.);
#3740=VECTOR('',#12396,1000.);
#3741=VECTOR('',#12399,1000.);
#3742=VECTOR('',#12402,1000.);
#3743=VECTOR('',#12405,1000.);
#3744=VECTOR('',#12408,1000.);
#3745=VECTOR('',#12411,1000.);
#3746=VECTOR('',#12414,1000.);
#3747=VECTOR('',#12417,1000.);
#3748=VECTOR('',#12420,1000.);
#3749=VECTOR('',#12423,1000.);
#3750=VECTOR('',#12426,1000.);
#3751=VECTOR('',#12429,1000.);
#3752=VECTOR('',#12432,1000.);
#3753=VECTOR('',#12435,1000.);
#3754=VECTOR('',#12438,1000.);
#3755=VECTOR('',#12441,1000.);
#3756=VECTOR('',#12444,1000.);
#3757=VECTOR('',#12447,1000.);
#3758=VECTOR('',#12450,1000.);
#3759=VECTOR('',#12453,1000.);
#3760=VECTOR('',#12456,1000.);
#3761=VECTOR('',#12459,1000.);
#3762=VECTOR('',#12462,1000.);
#3763=VECTOR('',#12465,1000.);
#3764=VECTOR('',#12468,1000.);
#3765=VECTOR('',#12471,1000.);
#3766=VECTOR('',#12474,1000.);
#3767=VECTOR('',#12477,1000.);
#3768=VECTOR('',#12480,1000.);
#3769=VECTOR('',#12483,1000.);
#3770=VECTOR('',#12486,1000.);
#3771=VECTOR('',#12489,1000.);
#3772=VECTOR('',#12492,1000.);
#3773=VECTOR('',#12495,1000.);
#3774=VECTOR('',#12498,1000.);
#3775=VECTOR('',#12501,1000.);
#3776=VECTOR('',#12504,1000.);
#3777=VECTOR('',#12507,1000.);
#3778=VECTOR('',#12510,1000.);
#3779=VECTOR('',#12513,1000.);
#3780=VECTOR('',#12516,1000.);
#3781=VECTOR('',#12519,1000.);
#3782=VECTOR('',#12522,1000.);
#3783=VECTOR('',#12525,1000.);
#3784=VECTOR('',#12534,1000.);
#3785=VECTOR('',#12535,1000.);
#3786=VECTOR('',#12536,1000.);
#3787=VECTOR('',#12539,1000.);
#3788=VECTOR('',#12540,1000.);
#3789=VECTOR('',#12541,1000.);
#3790=VECTOR('',#12544,1000.);
#3791=VECTOR('',#12547,1000.);
#3792=VECTOR('',#12552,1000.);
#3793=VECTOR('',#12553,1000.);
#3794=VECTOR('',#12554,1000.);
#3795=VECTOR('',#12557,1000.);
#3796=VECTOR('',#12558,1000.);
#3797=VECTOR('',#12559,1000.);
#3798=VECTOR('',#12562,1000.);
#3799=VECTOR('',#12565,1000.);
#3800=VECTOR('',#12570,1000.);
#3801=VECTOR('',#12571,1000.);
#3802=VECTOR('',#12572,1000.);
#3803=VECTOR('',#12575,1000.);
#3804=VECTOR('',#12576,1000.);
#3805=VECTOR('',#12577,1000.);
#3806=VECTOR('',#12580,1000.);
#3807=VECTOR('',#12583,1000.);
#3808=VECTOR('',#12588,1000.);
#3809=VECTOR('',#12589,1000.);
#3810=VECTOR('',#12590,1000.);
#3811=VECTOR('',#12593,1000.);
#3812=VECTOR('',#12594,1000.);
#3813=VECTOR('',#12595,1000.);
#3814=VECTOR('',#12598,1000.);
#3815=VECTOR('',#12601,1000.);
#3816=VECTOR('',#12606,1000.);
#3817=VECTOR('',#12607,1000.);
#3818=VECTOR('',#12608,1000.);
#3819=VECTOR('',#12611,1000.);
#3820=VECTOR('',#12612,1000.);
#3821=VECTOR('',#12613,1000.);
#3822=VECTOR('',#12616,1000.);
#3823=VECTOR('',#12619,1000.);
#3824=VECTOR('',#12624,1000.);
#3825=VECTOR('',#12625,1000.);
#3826=VECTOR('',#12626,1000.);
#3827=VECTOR('',#12629,1000.);
#3828=VECTOR('',#12630,1000.);
#3829=VECTOR('',#12631,1000.);
#3830=VECTOR('',#12634,1000.);
#3831=VECTOR('',#12637,1000.);
#3832=VECTOR('',#12642,1000.);
#3833=VECTOR('',#12643,1000.);
#3834=VECTOR('',#12644,1000.);
#3835=VECTOR('',#12647,1000.);
#3836=VECTOR('',#12648,1000.);
#3837=VECTOR('',#12649,1000.);
#3838=VECTOR('',#12652,1000.);
#3839=VECTOR('',#12655,1000.);
#3840=VECTOR('',#12660,1000.);
#3841=VECTOR('',#12661,1000.);
#3842=VECTOR('',#12662,1000.);
#3843=VECTOR('',#12665,1000.);
#3844=VECTOR('',#12666,1000.);
#3845=VECTOR('',#12667,1000.);
#3846=VECTOR('',#12670,1000.);
#3847=VECTOR('',#12673,1000.);
#3848=VECTOR('',#12678,1000.);
#3849=VECTOR('',#12679,1000.);
#3850=VECTOR('',#12680,1000.);
#3851=VECTOR('',#12683,1000.);
#3852=VECTOR('',#12684,1000.);
#3853=VECTOR('',#12685,1000.);
#3854=VECTOR('',#12688,1000.);
#3855=VECTOR('',#12691,1000.);
#3856=VECTOR('',#12696,1000.);
#3857=VECTOR('',#12697,1000.);
#3858=VECTOR('',#12698,1000.);
#3859=VECTOR('',#12701,1000.);
#3860=VECTOR('',#12702,1000.);
#3861=VECTOR('',#12703,1000.);
#3862=VECTOR('',#12706,1000.);
#3863=VECTOR('',#12709,1000.);
#3864=VECTOR('',#12714,1000.);
#3865=VECTOR('',#12715,1000.);
#3866=VECTOR('',#12716,1000.);
#3867=VECTOR('',#12719,1000.);
#3868=VECTOR('',#12720,1000.);
#3869=VECTOR('',#12721,1000.);
#3870=VECTOR('',#12724,1000.);
#3871=VECTOR('',#12727,1000.);
#3872=VECTOR('',#12732,1000.);
#3873=VECTOR('',#12733,1000.);
#3874=VECTOR('',#12734,1000.);
#3875=VECTOR('',#12737,1000.);
#3876=VECTOR('',#12738,1000.);
#3877=VECTOR('',#12739,1000.);
#3878=VECTOR('',#12742,1000.);
#3879=VECTOR('',#12745,1000.);
#3880=VECTOR('',#12750,1000.);
#3881=VECTOR('',#12751,1000.);
#3882=VECTOR('',#12752,1000.);
#3883=VECTOR('',#12755,1000.);
#3884=VECTOR('',#12756,1000.);
#3885=VECTOR('',#12757,1000.);
#3886=VECTOR('',#12760,1000.);
#3887=VECTOR('',#12763,1000.);
#3888=VECTOR('',#12768,1000.);
#3889=VECTOR('',#12769,1000.);
#3890=VECTOR('',#12770,1000.);
#3891=VECTOR('',#12773,1000.);
#3892=VECTOR('',#12774,1000.);
#3893=VECTOR('',#12775,1000.);
#3894=VECTOR('',#12778,1000.);
#3895=VECTOR('',#12781,1000.);
#3896=VECTOR('',#12786,1000.);
#3897=VECTOR('',#12787,1000.);
#3898=VECTOR('',#12788,1000.);
#3899=VECTOR('',#12791,1000.);
#3900=VECTOR('',#12792,1000.);
#3901=VECTOR('',#12793,1000.);
#3902=VECTOR('',#12796,1000.);
#3903=VECTOR('',#12799,1000.);
#3904=VECTOR('',#12804,1000.);
#3905=VECTOR('',#12805,1000.);
#3906=VECTOR('',#12806,1000.);
#3907=VECTOR('',#12809,1000.);
#3908=VECTOR('',#12810,1000.);
#3909=VECTOR('',#12811,1000.);
#3910=VECTOR('',#12814,1000.);
#3911=VECTOR('',#12817,1000.);
#3912=VECTOR('',#12822,1000.);
#3913=VECTOR('',#12823,1000.);
#3914=VECTOR('',#12824,1000.);
#3915=VECTOR('',#12827,1000.);
#3916=VECTOR('',#12828,1000.);
#3917=VECTOR('',#12829,1000.);
#3918=VECTOR('',#12832,1000.);
#3919=VECTOR('',#12835,1000.);
#3920=VECTOR('',#12840,1000.);
#3921=VECTOR('',#12841,1000.);
#3922=VECTOR('',#12842,1000.);
#3923=VECTOR('',#12845,1000.);
#3924=VECTOR('',#12846,1000.);
#3925=VECTOR('',#12847,1000.);
#3926=VECTOR('',#12850,1000.);
#3927=VECTOR('',#12853,1000.);
#3928=VECTOR('',#12858,1000.);
#3929=VECTOR('',#12859,1000.);
#3930=VECTOR('',#12860,1000.);
#3931=VECTOR('',#12863,1000.);
#3932=VECTOR('',#12864,1000.);
#3933=VECTOR('',#12865,1000.);
#3934=VECTOR('',#12868,1000.);
#3935=VECTOR('',#12871,1000.);
#3936=VECTOR('',#12876,1000.);
#3937=VECTOR('',#12877,1000.);
#3938=VECTOR('',#12878,1000.);
#3939=VECTOR('',#12881,1000.);
#3940=VECTOR('',#12882,1000.);
#3941=VECTOR('',#12883,1000.);
#3942=VECTOR('',#12886,1000.);
#3943=VECTOR('',#12889,1000.);
#3944=VECTOR('',#12894,1000.);
#3945=VECTOR('',#12895,1000.);
#3946=VECTOR('',#12896,1000.);
#3947=VECTOR('',#12899,1000.);
#3948=VECTOR('',#12900,1000.);
#3949=VECTOR('',#12901,1000.);
#3950=VECTOR('',#12904,1000.);
#3951=VECTOR('',#12907,1000.);
#3952=VECTOR('',#12912,1000.);
#3953=VECTOR('',#12913,1000.);
#3954=VECTOR('',#12914,1000.);
#3955=VECTOR('',#12917,1000.);
#3956=VECTOR('',#12918,1000.);
#3957=VECTOR('',#12919,1000.);
#3958=VECTOR('',#12922,1000.);
#3959=VECTOR('',#12925,1000.);
#3960=VECTOR('',#12930,1000.);
#3961=VECTOR('',#12931,1000.);
#3962=VECTOR('',#12932,1000.);
#3963=VECTOR('',#12935,1000.);
#3964=VECTOR('',#12936,1000.);
#3965=VECTOR('',#12937,1000.);
#3966=VECTOR('',#12940,1000.);
#3967=VECTOR('',#12943,1000.);
#3968=VECTOR('',#12948,1000.);
#3969=VECTOR('',#12949,1000.);
#3970=VECTOR('',#12950,1000.);
#3971=VECTOR('',#12953,1000.);
#3972=VECTOR('',#12954,1000.);
#3973=VECTOR('',#12955,1000.);
#3974=VECTOR('',#12958,1000.);
#3975=VECTOR('',#12961,1000.);
#3976=VECTOR('',#12966,1000.);
#3977=VECTOR('',#12967,1000.);
#3978=VECTOR('',#12968,1000.);
#3979=VECTOR('',#12971,1000.);
#3980=VECTOR('',#12972,1000.);
#3981=VECTOR('',#12973,1000.);
#3982=VECTOR('',#12976,1000.);
#3983=VECTOR('',#12979,1000.);
#3984=VECTOR('',#12984,1000.);
#3985=VECTOR('',#12985,1000.);
#3986=VECTOR('',#12986,1000.);
#3987=VECTOR('',#12989,1000.);
#3988=VECTOR('',#12990,1000.);
#3989=VECTOR('',#12991,1000.);
#3990=VECTOR('',#12994,1000.);
#3991=VECTOR('',#12997,1000.);
#3992=VECTOR('',#13002,1000.);
#3993=VECTOR('',#13003,1000.);
#3994=VECTOR('',#13004,1000.);
#3995=VECTOR('',#13007,1000.);
#3996=VECTOR('',#13008,1000.);
#3997=VECTOR('',#13009,1000.);
#3998=VECTOR('',#13012,1000.);
#3999=VECTOR('',#13015,1000.);
#4000=VECTOR('',#13020,1000.);
#4001=VECTOR('',#13021,1000.);
#4002=VECTOR('',#13022,1000.);
#4003=VECTOR('',#13025,1000.);
#4004=VECTOR('',#13026,1000.);
#4005=VECTOR('',#13027,1000.);
#4006=VECTOR('',#13030,1000.);
#4007=VECTOR('',#13033,1000.);
#4008=VECTOR('',#13038,1000.);
#4009=VECTOR('',#13039,1000.);
#4010=VECTOR('',#13040,1000.);
#4011=VECTOR('',#13043,1000.);
#4012=VECTOR('',#13044,1000.);
#4013=VECTOR('',#13045,1000.);
#4014=VECTOR('',#13048,1000.);
#4015=VECTOR('',#13051,1000.);
#4016=VECTOR('',#13056,1000.);
#4017=VECTOR('',#13057,1000.);
#4018=VECTOR('',#13058,1000.);
#4019=VECTOR('',#13061,1000.);
#4020=VECTOR('',#13062,1000.);
#4021=VECTOR('',#13063,1000.);
#4022=VECTOR('',#13066,1000.);
#4023=VECTOR('',#13069,1000.);
#4024=VECTOR('',#13074,1000.);
#4025=VECTOR('',#13075,1000.);
#4026=VECTOR('',#13076,1000.);
#4027=VECTOR('',#13079,1000.);
#4028=VECTOR('',#13080,1000.);
#4029=VECTOR('',#13081,1000.);
#4030=VECTOR('',#13084,1000.);
#4031=VECTOR('',#13087,1000.);
#4032=VECTOR('',#13092,1000.);
#4033=VECTOR('',#13093,1000.);
#4034=VECTOR('',#13094,1000.);
#4035=VECTOR('',#13097,1000.);
#4036=VECTOR('',#13098,1000.);
#4037=VECTOR('',#13099,1000.);
#4038=VECTOR('',#13102,1000.);
#4039=VECTOR('',#13105,1000.);
#4040=VECTOR('',#13110,1000.);
#4041=VECTOR('',#13111,1000.);
#4042=VECTOR('',#13112,1000.);
#4043=VECTOR('',#13115,1000.);
#4044=VECTOR('',#13116,1000.);
#4045=VECTOR('',#13117,1000.);
#4046=VECTOR('',#13120,1000.);
#4047=VECTOR('',#13123,1000.);
#4048=VECTOR('',#13128,1000.);
#4049=VECTOR('',#13129,1000.);
#4050=VECTOR('',#13130,1000.);
#4051=VECTOR('',#13133,1000.);
#4052=VECTOR('',#13134,1000.);
#4053=VECTOR('',#13135,1000.);
#4054=VECTOR('',#13138,1000.);
#4055=VECTOR('',#13141,1000.);
#4056=VECTOR('',#13146,1000.);
#4057=VECTOR('',#13147,1000.);
#4058=VECTOR('',#13148,1000.);
#4059=VECTOR('',#13151,1000.);
#4060=VECTOR('',#13152,1000.);
#4061=VECTOR('',#13153,1000.);
#4062=VECTOR('',#13156,1000.);
#4063=VECTOR('',#13159,1000.);
#4064=VECTOR('',#13164,1000.);
#4065=VECTOR('',#13165,1000.);
#4066=VECTOR('',#13166,1000.);
#4067=VECTOR('',#13169,1000.);
#4068=VECTOR('',#13170,1000.);
#4069=VECTOR('',#13171,1000.);
#4070=VECTOR('',#13174,1000.);
#4071=VECTOR('',#13177,1000.);
#4072=VECTOR('',#13182,1000.);
#4073=VECTOR('',#13183,1000.);
#4074=VECTOR('',#13184,1000.);
#4075=VECTOR('',#13187,1000.);
#4076=VECTOR('',#13188,1000.);
#4077=VECTOR('',#13189,1000.);
#4078=VECTOR('',#13192,1000.);
#4079=VECTOR('',#13195,1000.);
#4080=VECTOR('',#13200,1000.);
#4081=VECTOR('',#13201,1000.);
#4082=VECTOR('',#13202,1000.);
#4083=VECTOR('',#13205,1000.);
#4084=VECTOR('',#13206,1000.);
#4085=VECTOR('',#13207,1000.);
#4086=VECTOR('',#13210,1000.);
#4087=VECTOR('',#13213,1000.);
#4088=VECTOR('',#13218,1000.);
#4089=VECTOR('',#13219,1000.);
#4090=VECTOR('',#13220,1000.);
#4091=VECTOR('',#13223,1000.);
#4092=VECTOR('',#13224,1000.);
#4093=VECTOR('',#13225,1000.);
#4094=VECTOR('',#13228,1000.);
#4095=VECTOR('',#13231,1000.);
#4096=VECTOR('',#13236,1000.);
#4097=VECTOR('',#13237,1000.);
#4098=VECTOR('',#13238,1000.);
#4099=VECTOR('',#13241,1000.);
#4100=VECTOR('',#13242,1000.);
#4101=VECTOR('',#13243,1000.);
#4102=VECTOR('',#13246,1000.);
#4103=VECTOR('',#13249,1000.);
#4104=VECTOR('',#13258,3.2);
#4105=VECTOR('',#13265,4.2);
#4106=VECTOR('',#13270,1000.);
#4107=VECTOR('',#13271,1000.);
#4108=VECTOR('',#13272,1000.);
#4109=VECTOR('',#13273,1000.);
#4110=VECTOR('',#13274,1000.);
#4111=VECTOR('',#13275,1000.);
#4112=VECTOR('',#13276,1000.);
#4113=VECTOR('',#13277,1000.);
#4114=VECTOR('',#13278,1000.);
#4115=VECTOR('',#13279,1000.);
#4116=VECTOR('',#13280,1000.);
#4117=VECTOR('',#13281,1000.);
#4118=VECTOR('',#13282,1000.);
#4119=VECTOR('',#13283,1000.);
#4120=VECTOR('',#13286,1000.);
#4121=VECTOR('',#13287,1000.);
#4122=VECTOR('',#13288,1000.);
#4123=VECTOR('',#13289,1000.);
#4124=VECTOR('',#13290,1000.);
#4125=VECTOR('',#13291,1000.);
#4126=VECTOR('',#13292,1000.);
#4127=VECTOR('',#13293,1000.);
#4128=VECTOR('',#13294,1000.);
#4129=VECTOR('',#13295,1000.);
#4130=VECTOR('',#13296,1000.);
#4131=VECTOR('',#13297,1000.);
#4132=VECTOR('',#13298,1000.);
#4133=VECTOR('',#13299,1000.);
#4134=VECTOR('',#13302,1000.);
#4135=VECTOR('',#13303,1000.);
#4136=VECTOR('',#13306,1000.);
#4137=VECTOR('',#13309,1000.);
#4138=VECTOR('',#13312,1000.);
#4139=VECTOR('',#13315,1000.);
#4140=VECTOR('',#13318,1000.);
#4141=VECTOR('',#13321,1000.);
#4142=VECTOR('',#13324,1000.);
#4143=VECTOR('',#13327,1000.);
#4144=VECTOR('',#13330,1000.);
#4145=VECTOR('',#13333,1000.);
#4146=VECTOR('',#13336,1000.);
#4147=VECTOR('',#13339,1000.);
#4148=VECTOR('',#13348,7.5);
#4149=VECTOR('',#13357,9.);
#4150=VECTOR('',#13360,9.);
#4151=VECTOR('',#13367,3.2);
#4152=VECTOR('',#13380,5.);
#4153=VECTOR('',#13387,3.);
#4154=VECTOR('',#13402,4.2);
#4155=VECTOR('',#13407,1000.);
#4156=VECTOR('',#13408,1000.);
#4157=VECTOR('',#13409,1000.);
#4158=VECTOR('',#13410,1000.);
#4159=VECTOR('',#13411,1000.);
#4160=VECTOR('',#13412,1000.);
#4161=VECTOR('',#13415,1000.);
#4162=VECTOR('',#13416,1000.);
#4163=VECTOR('',#13417,1000.);
#4164=VECTOR('',#13418,1000.);
#4165=VECTOR('',#13419,1000.);
#4166=VECTOR('',#13420,1000.);
#4167=VECTOR('',#13423,1000.);
#4168=VECTOR('',#13424,1000.);
#4169=VECTOR('',#13427,1000.);
#4170=VECTOR('',#13430,1000.);
#4171=VECTOR('',#13433,1000.);
#4172=VECTOR('',#13436,1000.);
#4173=VECTOR('',#13445,2.4);
#4174=VECTOR('',#13452,5.);
#4175=VECTOR('',#13457,1000.);
#4176=VECTOR('',#13458,1000.);
#4177=VECTOR('',#13459,1000.);
#4178=VECTOR('',#13460,1000.);
#4179=VECTOR('',#13461,1000.);
#4180=VECTOR('',#13462,1000.);
#4181=VECTOR('',#13469,1000.);
#4182=VECTOR('',#13470,1000.);
#4183=VECTOR('',#13471,1000.);
#4184=VECTOR('',#13474,1000.);
#4185=VECTOR('',#13475,1000.);
#4186=VECTOR('',#13478,1000.);
#4187=VECTOR('',#13479,1000.);
#4188=VECTOR('',#13482,1000.);
#4189=VECTOR('',#13483,1000.);
#4190=VECTOR('',#13486,1000.);
#4191=VECTOR('',#13487,1000.);
#4192=VECTOR('',#13490,1000.);
#4193=VECTOR('',#13499,2.);
#4194=VECTOR('',#13504,1000.);
#4195=VECTOR('',#13505,1000.);
#4196=VECTOR('',#13506,1000.);
#4197=VECTOR('',#13507,1000.);
#4198=VECTOR('',#13510,1000.);
#4199=VECTOR('',#13511,1000.);
#4200=VECTOR('',#13512,1000.);
#4201=VECTOR('',#13515,1000.);
#4202=VECTOR('',#13516,1000.);
#4203=VECTOR('',#13517,1000.);
#4204=VECTOR('',#13520,1000.);
#4205=VECTOR('',#13521,1000.);
#4206=VECTOR('',#13522,1000.);
#4207=VECTOR('',#13525,1000.);
#4208=VECTOR('',#13526,1000.);
#4209=VECTOR('',#13527,1000.);
#4210=VECTOR('',#13530,1000.);
#4211=VECTOR('',#13531,1000.);
#4212=VECTOR('',#13544,1.5);
#4213=VECTOR('',#13551,3.5);
#4214=VECTOR('',#13556,1000.);
#4215=VECTOR('',#13557,1000.);
#4216=VECTOR('',#13558,1000.);
#4217=VECTOR('',#13559,1000.);
#4218=VECTOR('',#13560,1000.);
#4219=VECTOR('',#13561,1000.);
#4220=VECTOR('',#13568,1000.);
#4221=VECTOR('',#13569,1000.);
#4222=VECTOR('',#13570,1000.);
#4223=VECTOR('',#13573,1000.);
#4224=VECTOR('',#13574,1000.);
#4225=VECTOR('',#13577,1000.);
#4226=VECTOR('',#13578,1000.);
#4227=VECTOR('',#13581,1000.);
#4228=VECTOR('',#13582,1000.);
#4229=VECTOR('',#13585,1000.);
#4230=VECTOR('',#13586,1000.);
#4231=VECTOR('',#13589,1000.);
#4232=CIRCLE('',#10079,2.5);
#4233=CIRCLE('',#10080,2.5);
#4234=CIRCLE('',#10082,2.5);
#4235=CIRCLE('',#10083,2.5);
#4236=CIRCLE('',#10096,14.2);
#4237=CIRCLE('',#10130,14.2);
#4238=CIRCLE('',#10134,14.2);
#4239=CIRCLE('',#10135,14.2);
#4240=CIRCLE('',#10137,2.5);
#4241=CIRCLE('',#10138,2.5);
#4242=CIRCLE('',#10140,2.5);
#4243=CIRCLE('',#10141,2.5);
#4244=CIRCLE('',#10143,2.6);
#4245=CIRCLE('',#10145,2.6);
#4246=CIRCLE('',#10148,2.6);
#4247=CIRCLE('',#10150,2.6);
#4248=CIRCLE('',#10153,2.6);
#4249=CIRCLE('',#10155,2.6);
#4250=CIRCLE('',#10191,2.59999999999999);
#4251=CIRCLE('',#10192,2.6);
#4252=CIRCLE('',#10194,2.6);
#4253=CIRCLE('',#10196,2.59999999999999);
#4254=CIRCLE('',#10197,2.6);
#4255=CIRCLE('',#10199,2.6);
#4256=CIRCLE('',#10201,2.59999999999999);
#4257=CIRCLE('',#10202,2.6);
#4258=CIRCLE('',#10204,2.6);
#4259=CIRCLE('',#10206,2.5);
#4260=CIRCLE('',#10207,2.5);
#4261=CIRCLE('',#10209,2.5);
#4262=CIRCLE('',#10210,2.5);
#4263=CIRCLE('',#10212,9.1);
#4264=CIRCLE('',#10213,9.1);
#4265=CIRCLE('',#10268,1.65);
#4266=CIRCLE('',#10269,1.65);
#4267=CIRCLE('',#10271,1.65);
#4268=CIRCLE('',#10272,1.65);
#4269=CIRCLE('',#10274,2.5);
#4270=CIRCLE('',#10275,2.5);
#4271=CIRCLE('',#10277,2.5);
#4272=CIRCLE('',#10278,2.5);
#4273=CIRCLE('',#10280,6.15);
#4274=CIRCLE('',#10281,6.15);
#4275=CIRCLE('',#10315,3.7);
#4276=CIRCLE('',#10316,3.7);
#4277=CIRCLE('',#10318,3.7);
#4278=CIRCLE('',#10319,3.7);
#4279=CIRCLE('',#10321,2.2);
#4280=CIRCLE('',#10322,2.2);
#4281=CIRCLE('',#10324,2.2);
#4282=CIRCLE('',#10325,2.2);
#4283=CIRCLE('',#10336,5.55);
#4284=CIRCLE('',#10337,5.55);
#4285=CIRCLE('',#10339,6.);
#4286=CIRCLE('',#10340,6.);
#4287=CIRCLE('',#10342,9.);
#4288=CIRCLE('',#10343,9.);
#4289=CIRCLE('',#10345,6.);
#4290=CIRCLE('',#10346,6.);
#4291=CIRCLE('',#10348,4.);
#4292=CIRCLE('',#10349,4.);
#4293=CIRCLE('',#10358,7.15);
#4294=CIRCLE('',#10359,7.15);
#4295=CIRCLE('',#10361,6.);
#4296=CIRCLE('',#10362,6.);
#4297=CIRCLE('',#10364,9.);
#4298=CIRCLE('',#10365,9.);
#4299=CIRCLE('',#10367,6.);
#4300=CIRCLE('',#10368,6.);
#4301=CIRCLE('',#10370,4.);
#4302=CIRCLE('',#10371,4.);
#4303=CIRCLE('',#10380,2.2);
#4304=CIRCLE('',#10382,2.2);
#4305=CIRCLE('',#10384,6.);
#4306=CIRCLE('',#10385,6.);
#4307=CIRCLE('',#10387,8.75);
#4308=CIRCLE('',#10388,8.75);
#4309=CIRCLE('',#10390,10.);
#4310=CIRCLE('',#10391,10.);
#4311=CIRCLE('',#10392,10.);
#4312=CIRCLE('',#10393,10.);
#4313=CIRCLE('',#10394,10.);
#4314=CIRCLE('',#10395,10.);
#4315=CIRCLE('',#10406,5.75);
#4316=CIRCLE('',#10407,5.75);
#4317=CIRCLE('',#10416,7.35);
#4318=CIRCLE('',#10417,7.35);
#4319=CIRCLE('',#10426,2.19999999999999);
#4320=CIRCLE('',#10427,2.19999999999999);
#4321=CIRCLE('',#10429,7.00000000000001);
#4322=CIRCLE('',#10430,7.00000000000001);
#4323=CIRCLE('',#10432,5.);
#4324=CIRCLE('',#10433,5.);
#4325=CIRCLE('',#10435,3.);
#4326=CIRCLE('',#10442,2.);
#4327=CIRCLE('',#10443,2.);
#4328=CIRCLE('',#10448,5.50000000000001);
#4329=CIRCLE('',#10449,5.50000000000001);
#4330=CIRCLE('',#10451,5.50000000000001);
#4331=CIRCLE('',#10452,5.50000000000001);
#4332=CIRCLE('',#10454,3.3);
#4333=CIRCLE('',#10455,3.3);
#4334=CIRCLE('',#10457,3.3);
#4335=CIRCLE('',#10458,3.3);
#4336=CIRCLE('',#10469,3.3);
#4337=CIRCLE('',#10470,3.3);
#4338=CIRCLE('',#10472,3.3);
#4339=CIRCLE('',#10473,3.3);
#4340=CIRCLE('',#10475,6.2);
#4341=CIRCLE('',#10476,6.2);
#4342=CIRCLE('',#10489,6.2);
#4343=CIRCLE('',#10490,6.2);
#4344=CIRCLE('',#10492,14.);
#4345=CIRCLE('',#10493,14.);
#4346=CIRCLE('',#10494,14.);
#4347=CIRCLE('',#10495,14.);
#4348=CIRCLE('',#10496,14.);
#4349=CIRCLE('',#10497,14.);
#4350=CIRCLE('',#10498,14.);
#4351=CIRCLE('',#10499,14.);
#4352=CIRCLE('',#10500,14.);
#4353=CIRCLE('',#10501,14.);
#4354=CIRCLE('',#10502,14.);
#4355=CIRCLE('',#10503,14.);
#4356=CIRCLE('',#10504,14.);
#4357=CIRCLE('',#10505,14.);
#4358=CIRCLE('',#10506,14.);
#4359=CIRCLE('',#10507,14.);
#4360=CIRCLE('',#10508,14.);
#4361=CIRCLE('',#10509,14.);
#4362=CIRCLE('',#10510,14.);
#4363=CIRCLE('',#10511,14.);
#4364=CIRCLE('',#10512,14.);
#4365=CIRCLE('',#10513,14.);
#4366=CIRCLE('',#10514,14.);
#4367=CIRCLE('',#10515,14.);
#4368=CIRCLE('',#10516,14.);
#4369=CIRCLE('',#10517,14.);
#4370=CIRCLE('',#10518,14.);
#4371=CIRCLE('',#10519,14.);
#4372=CIRCLE('',#10520,14.);
#4373=CIRCLE('',#10521,14.);
#4374=CIRCLE('',#10522,14.);
#4375=CIRCLE('',#10523,14.);
#4376=CIRCLE('',#10524,14.);
#4377=CIRCLE('',#10525,14.);
#4378=CIRCLE('',#10526,14.);
#4379=CIRCLE('',#10527,14.);
#4380=CIRCLE('',#10528,14.);
#4381=CIRCLE('',#10529,14.);
#4382=CIRCLE('',#10530,14.);
#4383=CIRCLE('',#10531,14.);
#4384=CIRCLE('',#10532,14.);
#4385=CIRCLE('',#10533,14.);
#4386=CIRCLE('',#10534,14.);
#4387=CIRCLE('',#10535,14.);
#4388=CIRCLE('',#10536,14.);
#4389=CIRCLE('',#10537,14.);
#4390=CIRCLE('',#10538,14.);
#4391=CIRCLE('',#10539,14.);
#4392=CIRCLE('',#10540,14.);
#4393=CIRCLE('',#10541,14.);
#4394=CIRCLE('',#10542,14.);
#4395=CIRCLE('',#10543,14.);
#4396=CIRCLE('',#10544,14.);
#4397=CIRCLE('',#10545,14.);
#4398=CIRCLE('',#10546,14.);
#4399=CIRCLE('',#10547,14.);
#4400=CIRCLE('',#10548,14.);
#4401=CIRCLE('',#10549,14.);
#4402=CIRCLE('',#10550,14.);
#4403=CIRCLE('',#10551,14.);
#4404=CIRCLE('',#10552,14.);
#4405=CIRCLE('',#10553,14.);
#4406=CIRCLE('',#10554,14.);
#4407=CIRCLE('',#10555,14.);
#4408=CIRCLE('',#10556,14.);
#4409=CIRCLE('',#10557,14.);
#4410=CIRCLE('',#10558,14.);
#4411=CIRCLE('',#10559,14.);
#4412=CIRCLE('',#10560,14.);
#4413=CIRCLE('',#10561,14.);
#4414=CIRCLE('',#10562,14.);
#4415=CIRCLE('',#10563,14.);
#4416=CIRCLE('',#10564,14.);
#4417=CIRCLE('',#10565,14.);
#4418=CIRCLE('',#10566,14.);
#4419=CIRCLE('',#10567,14.);
#4420=CIRCLE('',#10568,14.);
#4421=CIRCLE('',#10569,14.);
#4422=CIRCLE('',#10570,14.);
#4423=CIRCLE('',#10571,14.);
#4424=CIRCLE('',#10572,14.);
#4425=CIRCLE('',#10573,14.);
#4426=CIRCLE('',#10574,14.);
#4427=CIRCLE('',#10575,14.);
#4428=CIRCLE('',#10780,3.2);
#4429=CIRCLE('',#10781,3.2);
#4430=CIRCLE('',#10783,4.2);
#4431=CIRCLE('',#10784,4.2);
#4432=CIRCLE('',#10803,9.);
#4433=CIRCLE('',#10804,7.5);
#4434=CIRCLE('',#10806,9.);
#4435=CIRCLE('',#10807,9.);
#4436=CIRCLE('',#10809,8.);
#4437=CIRCLE('',#10811,3.2);
#4438=CIRCLE('',#10812,3.2);
#4439=CIRCLE('',#10817,5.);
#4440=CIRCLE('',#10818,5.);
#4441=CIRCLE('',#10820,3.);
#4442=CIRCLE('',#10821,3.);
#4443=CIRCLE('',#10827,4.2);
#4444=CIRCLE('',#10828,4.2);
#4445=CIRCLE('',#10839,2.4);
#4446=CIRCLE('',#10840,2.4);
#4447=CIRCLE('',#10842,5.);
#4448=CIRCLE('',#10843,5.);
#4449=CIRCLE('',#10856,2.);
#4450=CIRCLE('',#10857,2.);
#4451=CIRCLE('',#10869,1.5);
#4452=CIRCLE('',#10870,1.5);
#4453=CIRCLE('',#10872,3.5);
#4454=CIRCLE('',#10873,3.5);
#4455=VERTEX_POINT('',#13683);
#4456=VERTEX_POINT('',#13685);
#4457=VERTEX_POINT('',#13689);
#4458=VERTEX_POINT('',#13691);
#4459=VERTEX_POINT('',#13695);
#4460=VERTEX_POINT('',#13696);
#4461=VERTEX_POINT('',#13698);
#4462=VERTEX_POINT('',#13700);
#4463=VERTEX_POINT('',#13702);
#4464=VERTEX_POINT('',#13704);
#4465=VERTEX_POINT('',#13706);
#4466=VERTEX_POINT('',#13708);
#4467=VERTEX_POINT('',#13710);
#4468=VERTEX_POINT('',#13712);
#4469=VERTEX_POINT('',#13714);
#4470=VERTEX_POINT('',#13716);
#4471=VERTEX_POINT('',#13718);
#4472=VERTEX_POINT('',#13720);
#4473=VERTEX_POINT('',#13722);
#4474=VERTEX_POINT('',#13724);
#4475=VERTEX_POINT('',#13726);
#4476=VERTEX_POINT('',#13728);
#4477=VERTEX_POINT('',#13730);
#4478=VERTEX_POINT('',#13732);
#4479=VERTEX_POINT('',#13734);
#4480=VERTEX_POINT('',#13736);
#4481=VERTEX_POINT('',#13738);
#4482=VERTEX_POINT('',#13740);
#4483=VERTEX_POINT('',#13742);
#4484=VERTEX_POINT('',#13744);
#4485=VERTEX_POINT('',#13746);
#4486=VERTEX_POINT('',#13748);
#4487=VERTEX_POINT('',#13750);
#4488=VERTEX_POINT('',#13752);
#4489=VERTEX_POINT('',#13754);
#4490=VERTEX_POINT('',#13756);
#4491=VERTEX_POINT('',#13759);
#4492=VERTEX_POINT('',#13760);
#4493=VERTEX_POINT('',#13762);
#4494=VERTEX_POINT('',#13764);
#4495=VERTEX_POINT('',#13767);
#4496=VERTEX_POINT('',#13768);
#4497=VERTEX_POINT('',#13770);
#4498=VERTEX_POINT('',#13772);
#4499=VERTEX_POINT('',#13776);
#4500=VERTEX_POINT('',#13778);
#4501=VERTEX_POINT('',#13782);
#4502=VERTEX_POINT('',#13784);
#4503=VERTEX_POINT('',#13788);
#4504=VERTEX_POINT('',#13790);
#4505=VERTEX_POINT('',#13794);
#4506=VERTEX_POINT('',#13796);
#4507=VERTEX_POINT('',#13800);
#4508=VERTEX_POINT('',#13802);
#4509=VERTEX_POINT('',#13806);
#4510=VERTEX_POINT('',#13808);
#4511=VERTEX_POINT('',#13812);
#4512=VERTEX_POINT('',#13814);
#4513=VERTEX_POINT('',#13818);
#4514=VERTEX_POINT('',#13820);
#4515=VERTEX_POINT('',#13824);
#4516=VERTEX_POINT('',#13826);
#4517=VERTEX_POINT('',#13829);
#4518=VERTEX_POINT('',#13831);
#4519=VERTEX_POINT('',#13834);
#4520=VERTEX_POINT('',#13836);
#4521=VERTEX_POINT('',#13840);
#4522=VERTEX_POINT('',#13842);
#4523=VERTEX_POINT('',#13845);
#4524=VERTEX_POINT('',#13847);
#4525=VERTEX_POINT('',#13850);
#4526=VERTEX_POINT('',#13852);
#4527=VERTEX_POINT('',#13860);
#4528=VERTEX_POINT('',#13862);
#4529=VERTEX_POINT('',#13866);
#4530=VERTEX_POINT('',#13868);
#4531=VERTEX_POINT('',#13872);
#4532=VERTEX_POINT('',#13874);
#4533=VERTEX_POINT('',#13883);
#4534=VERTEX_POINT('',#13885);
#4535=VERTEX_POINT('',#13889);
#4536=VERTEX_POINT('',#13891);
#4537=VERTEX_POINT('',#13895);
#4538=VERTEX_POINT('',#13897);
#4539=VERTEX_POINT('',#13942);
#4540=VERTEX_POINT('',#13943);
#4541=VERTEX_POINT('',#13945);
#4542=VERTEX_POINT('',#13947);
#4543=VERTEX_POINT('',#13951);
#4544=VERTEX_POINT('',#13953);
#4545=VERTEX_POINT('',#13957);
#4546=VERTEX_POINT('',#13959);
#4547=VERTEX_POINT('',#13963);
#4548=VERTEX_POINT('',#13965);
#4549=VERTEX_POINT('',#13967);
#4550=VERTEX_POINT('',#13969);
#4551=VERTEX_POINT('',#13973);
#4552=VERTEX_POINT('',#13975);
#4553=VERTEX_POINT('',#13977);
#4554=VERTEX_POINT('',#13979);
#4555=VERTEX_POINT('',#13983);
#4556=VERTEX_POINT('',#13985);
#4557=VERTEX_POINT('',#13987);
#4558=VERTEX_POINT('',#13989);
#4559=VERTEX_POINT('',#13994);
#4560=VERTEX_POINT('',#13996);
#4561=VERTEX_POINT('',#13998);
#4562=VERTEX_POINT('',#14000);
#4563=VERTEX_POINT('',#14003);
#4564=VERTEX_POINT('',#14004);
#4565=VERTEX_POINT('',#14006);
#4566=VERTEX_POINT('',#14008);
#4567=VERTEX_POINT('',#14011);
#4568=VERTEX_POINT('',#14012);
#4569=VERTEX_POINT('',#14014);
#4570=VERTEX_POINT('',#14016);
#4571=VERTEX_POINT('',#14020);
#4572=VERTEX_POINT('',#14021);
#4573=VERTEX_POINT('',#14023);
#4574=VERTEX_POINT('',#14025);
#4575=VERTEX_POINT('',#14032);
#4576=VERTEX_POINT('',#14034);
#4577=VERTEX_POINT('',#14038);
#4578=VERTEX_POINT('',#14040);
#4579=VERTEX_POINT('',#14044);
#4580=VERTEX_POINT('',#14046);
#4581=VERTEX_POINT('',#14050);
#4582=VERTEX_POINT('',#14052);
#4583=VERTEX_POINT('',#14056);
#4584=VERTEX_POINT('',#14058);
#4585=VERTEX_POINT('',#14065);
#4586=VERTEX_POINT('',#14067);
#4587=VERTEX_POINT('',#14071);
#4588=VERTEX_POINT('',#14073);
#4589=VERTEX_POINT('',#14077);
#4590=VERTEX_POINT('',#14079);
#4591=VERTEX_POINT('',#14088);
#4592=VERTEX_POINT('',#14090);
#4593=VERTEX_POINT('',#14094);
#4594=VERTEX_POINT('',#14096);
#4595=VERTEX_POINT('',#14100);
#4596=VERTEX_POINT('',#14102);
#4597=VERTEX_POINT('',#14111);
#4598=VERTEX_POINT('',#14113);
#4599=VERTEX_POINT('',#14117);
#4600=VERTEX_POINT('',#14119);
#4601=VERTEX_POINT('',#14123);
#4602=VERTEX_POINT('',#14125);
#4603=VERTEX_POINT('',#14141);
#4604=VERTEX_POINT('',#14143);
#4605=VERTEX_POINT('',#14145);
#4606=VERTEX_POINT('',#14147);
#4607=VERTEX_POINT('',#14151);
#4608=VERTEX_POINT('',#14153);
#4609=VERTEX_POINT('',#14155);
#4610=VERTEX_POINT('',#14157);
#4611=VERTEX_POINT('',#14161);
#4612=VERTEX_POINT('',#14163);
#4613=VERTEX_POINT('',#14165);
#4614=VERTEX_POINT('',#14167);
#4615=VERTEX_POINT('',#14171);
#4616=VERTEX_POINT('',#14173);
#4617=VERTEX_POINT('',#14177);
#4618=VERTEX_POINT('',#14179);
#4619=VERTEX_POINT('',#14183);
#4620=VERTEX_POINT('',#14185);
#4621=VERTEX_POINT('',#14189);
#4622=VERTEX_POINT('',#14190);
#4623=VERTEX_POINT('',#14192);
#4624=VERTEX_POINT('',#14194);
#4625=VERTEX_POINT('',#14196);
#4626=VERTEX_POINT('',#14198);
#4627=VERTEX_POINT('',#14200);
#4628=VERTEX_POINT('',#14202);
#4629=VERTEX_POINT('',#14204);
#4630=VERTEX_POINT('',#14206);
#4631=VERTEX_POINT('',#14208);
#4632=VERTEX_POINT('',#14210);
#4633=VERTEX_POINT('',#14213);
#4634=VERTEX_POINT('',#14214);
#4635=VERTEX_POINT('',#14216);
#4636=VERTEX_POINT('',#14218);
#4637=VERTEX_POINT('',#14220);
#4638=VERTEX_POINT('',#14222);
#4639=VERTEX_POINT('',#14224);
#4640=VERTEX_POINT('',#14226);
#4641=VERTEX_POINT('',#14228);
#4642=VERTEX_POINT('',#14230);
#4643=VERTEX_POINT('',#14232);
#4644=VERTEX_POINT('',#14234);
#4645=VERTEX_POINT('',#14238);
#4646=VERTEX_POINT('',#14239);
#4647=VERTEX_POINT('',#14241);
#4648=VERTEX_POINT('',#14243);
#4649=VERTEX_POINT('',#14245);
#4650=VERTEX_POINT('',#14247);
#4651=VERTEX_POINT('',#14249);
#4652=VERTEX_POINT('',#14251);
#4653=VERTEX_POINT('',#14253);
#4654=VERTEX_POINT('',#14255);
#4655=VERTEX_POINT('',#14257);
#4656=VERTEX_POINT('',#14259);
#4657=VERTEX_POINT('',#14263);
#4658=VERTEX_POINT('',#14265);
#4659=VERTEX_POINT('',#14268);
#4660=VERTEX_POINT('',#14270);
#4661=VERTEX_POINT('',#14274);
#4662=VERTEX_POINT('',#14276);
#4663=VERTEX_POINT('',#14280);
#4664=VERTEX_POINT('',#14281);
#4665=VERTEX_POINT('',#14286);
#4666=VERTEX_POINT('',#14287);
#4667=VERTEX_POINT('',#14292);
#4668=VERTEX_POINT('',#14294);
#4669=VERTEX_POINT('',#14298);
#4670=VERTEX_POINT('',#14300);
#4671=VERTEX_POINT('',#14304);
#4672=VERTEX_POINT('',#14305);
#4673=VERTEX_POINT('',#14310);
#4674=VERTEX_POINT('',#14311);
#4675=VERTEX_POINT('',#14313);
#4676=VERTEX_POINT('',#14315);
#4677=VERTEX_POINT('',#14319);
#4678=VERTEX_POINT('',#14320);
#4679=VERTEX_POINT('',#14322);
#4680=VERTEX_POINT('',#14324);
#4681=VERTEX_POINT('',#14328);
#4682=VERTEX_POINT('',#14329);
#4683=VERTEX_POINT('',#14334);
#4684=VERTEX_POINT('',#14336);
#4685=VERTEX_POINT('',#14340);
#4686=VERTEX_POINT('',#14342);
#4687=VERTEX_POINT('',#14349);
#4688=VERTEX_POINT('',#14350);
#4689=VERTEX_POINT('',#14352);
#4690=VERTEX_POINT('',#14360);
#4691=VERTEX_POINT('',#14364);
#4692=VERTEX_POINT('',#14368);
#4693=VERTEX_POINT('',#14373);
#4694=VERTEX_POINT('',#14375);
#4695=VERTEX_POINT('',#14381);
#4696=VERTEX_POINT('',#14383);
#4697=VERTEX_POINT('',#14385);
#4698=VERTEX_POINT('',#14387);
#4699=VERTEX_POINT('',#14393);
#4700=VERTEX_POINT('',#14395);
#4701=VERTEX_POINT('',#14397);
#4702=VERTEX_POINT('',#14399);
#4703=VERTEX_POINT('',#14403);
#4704=VERTEX_POINT('',#14407);
#4705=VERTEX_POINT('',#14411);
#4706=VERTEX_POINT('',#14415);
#4707=VERTEX_POINT('',#14422);
#4708=VERTEX_POINT('',#14426);
#4709=VERTEX_POINT('',#14430);
#4710=VERTEX_POINT('',#14434);
#4711=VERTEX_POINT('',#14450);
#4712=VERTEX_POINT('',#14456);
#4713=VERTEX_POINT('',#14475);
#4714=VERTEX_POINT('',#14477);
#4715=VERTEX_POINT('',#14481);
#4716=VERTEX_POINT('',#14483);
#4717=VERTEX_POINT('',#14487);
#4718=VERTEX_POINT('',#14489);
#4719=VERTEX_POINT('',#14493);
#4720=VERTEX_POINT('',#14495);
#4721=VERTEX_POINT('',#14499);
#4722=VERTEX_POINT('',#14501);
#4723=VERTEX_POINT('',#14505);
#4724=VERTEX_POINT('',#14506);
#4725=VERTEX_POINT('',#14508);
#4726=VERTEX_POINT('',#14510);
#4727=VERTEX_POINT('',#14514);
#4728=VERTEX_POINT('',#14515);
#4729=VERTEX_POINT('',#14517);
#4730=VERTEX_POINT('',#14519);
#4731=VERTEX_POINT('',#14523);
#4732=VERTEX_POINT('',#14525);
#4733=VERTEX_POINT('',#14529);
#4734=VERTEX_POINT('',#14531);
#4735=VERTEX_POINT('',#14535);
#4736=VERTEX_POINT('',#14537);
#4737=VERTEX_POINT('',#14541);
#4738=VERTEX_POINT('',#14543);
#4739=VERTEX_POINT('',#14550);
#4740=VERTEX_POINT('',#14552);
#4741=VERTEX_POINT('',#14556);
#4742=VERTEX_POINT('',#14558);
#4743=VERTEX_POINT('',#14573);
#4744=VERTEX_POINT('',#14574);
#4745=VERTEX_POINT('',#14576);
#4746=VERTEX_POINT('',#14578);
#4747=VERTEX_POINT('',#14582);
#4748=VERTEX_POINT('',#14584);
#4749=VERTEX_POINT('',#14588);
#4750=VERTEX_POINT('',#14590);
#4751=VERTEX_POINT('',#14600);
#4752=VERTEX_POINT('',#14601);
#4753=VERTEX_POINT('',#14603);
#4754=VERTEX_POINT('',#14605);
#4755=VERTEX_POINT('',#14609);
#4756=VERTEX_POINT('',#14611);
#4757=VERTEX_POINT('',#14615);
#4758=VERTEX_POINT('',#14617);
#4759=VERTEX_POINT('',#14627);
#4760=VERTEX_POINT('',#14629);
#4761=VERTEX_POINT('',#14633);
#4762=VERTEX_POINT('',#14635);
#4763=VERTEX_POINT('',#14639);
#4764=VERTEX_POINT('',#14641);
#4765=VERTEX_POINT('',#14645);
#4766=VERTEX_POINT('',#14647);
#4767=VERTEX_POINT('',#14651);
#4768=VERTEX_POINT('',#14652);
#4769=VERTEX_POINT('',#14654);
#4770=VERTEX_POINT('',#14656);
#4771=VERTEX_POINT('',#14660);
#4772=VERTEX_POINT('',#14662);
#4773=VERTEX_POINT('',#14666);
#4774=VERTEX_POINT('',#14668);
#4775=VERTEX_POINT('',#14680);
#4776=VERTEX_POINT('',#14682);
#4777=VERTEX_POINT('',#14686);
#4778=VERTEX_POINT('',#14688);
#4779=VERTEX_POINT('',#14692);
#4780=VERTEX_POINT('',#14694);
#4781=VERTEX_POINT('',#14698);
#4782=VERTEX_POINT('',#14700);
#4783=VERTEX_POINT('',#14704);
#4784=VERTEX_POINT('',#14706);
#4785=VERTEX_POINT('',#14717);
#4786=VERTEX_POINT('',#14719);
#4787=VERTEX_POINT('',#14723);
#4788=VERTEX_POINT('',#14725);
#4789=VERTEX_POINT('',#14729);
#4790=VERTEX_POINT('',#14731);
#4791=VERTEX_POINT('',#14735);
#4792=VERTEX_POINT('',#14737);
#4793=VERTEX_POINT('',#14741);
#4794=VERTEX_POINT('',#14743);
#4795=VERTEX_POINT('',#14754);
#4796=VERTEX_POINT('',#14756);
#4797=VERTEX_POINT('',#14758);
#4798=VERTEX_POINT('',#14797);
#4799=VERTEX_POINT('',#14798);
#4800=VERTEX_POINT('',#14817);
#4801=VERTEX_POINT('',#14840);
#4802=VERTEX_POINT('',#14842);
#4803=VERTEX_POINT('',#14846);
#4804=VERTEX_POINT('',#14848);
#4805=VERTEX_POINT('',#14852);
#4806=VERTEX_POINT('',#14853);
#4807=VERTEX_POINT('',#14855);
#4808=VERTEX_POINT('',#14857);
#4809=VERTEX_POINT('',#14859);
#4810=VERTEX_POINT('',#14861);
#4811=VERTEX_POINT('',#14864);
#4812=VERTEX_POINT('',#14867);
#4813=VERTEX_POINT('',#14869);
#4814=VERTEX_POINT('',#14871);
#4815=VERTEX_POINT('',#14888);
#4816=VERTEX_POINT('',#14890);
#4817=VERTEX_POINT('',#14894);
#4818=VERTEX_POINT('',#14895);
#4819=VERTEX_POINT('',#14897);
#4820=VERTEX_POINT('',#14899);
#4821=VERTEX_POINT('',#14903);
#4822=VERTEX_POINT('',#14904);
#4823=VERTEX_POINT('',#14906);
#4824=VERTEX_POINT('',#14908);
#4825=VERTEX_POINT('',#14921);
#4826=VERTEX_POINT('',#14923);
#4827=VERTEX_POINT('',#14927);
#4828=VERTEX_POINT('',#14928);
#4829=VERTEX_POINT('',#14930);
#4830=VERTEX_POINT('',#14932);
#4831=VERTEX_POINT('',#14936);
#4832=VERTEX_POINT('',#14937);
#4833=VERTEX_POINT('',#14939);
#4834=VERTEX_POINT('',#14941);
#4835=VERTEX_POINT('',#14954);
#4836=VERTEX_POINT('',#14956);
#4837=VERTEX_POINT('',#14960);
#4838=VERTEX_POINT('',#14962);
#4839=VERTEX_POINT('',#15002);
#4840=VERTEX_POINT('',#15004);
#4841=VERTEX_POINT('',#15008);
#4842=VERTEX_POINT('',#15017);
#4843=VERTEX_POINT('',#15019);
#4844=VERTEX_POINT('',#15026);
#4845=VERTEX_POINT('',#15028);
#4846=VERTEX_POINT('',#15032);
#4847=VERTEX_POINT('',#15034);
#4848=VERTEX_POINT('',#15038);
#4849=VERTEX_POINT('',#15040);
#4850=VERTEX_POINT('',#15044);
#4851=VERTEX_POINT('',#15046);
#4852=VERTEX_POINT('',#15050);
#4853=VERTEX_POINT('',#15051);
#4854=VERTEX_POINT('',#15053);
#4855=VERTEX_POINT('',#15055);
#4856=VERTEX_POINT('',#15059);
#4857=VERTEX_POINT('',#15061);
#4858=VERTEX_POINT('',#15065);
#4859=VERTEX_POINT('',#15067);
#4860=VERTEX_POINT('',#15079);
#4861=VERTEX_POINT('',#15081);
#4862=VERTEX_POINT('',#15085);
#4863=VERTEX_POINT('',#15087);
#4864=VERTEX_POINT('',#15091);
#4865=VERTEX_POINT('',#15093);
#4866=VERTEX_POINT('',#15097);
#4867=VERTEX_POINT('',#15098);
#4868=VERTEX_POINT('',#15100);
#4869=VERTEX_POINT('',#15102);
#4870=VERTEX_POINT('',#15104);
#4871=VERTEX_POINT('',#15106);
#4872=VERTEX_POINT('',#15108);
#4873=VERTEX_POINT('',#15110);
#4874=VERTEX_POINT('',#15114);
#4875=VERTEX_POINT('',#15115);
#4876=VERTEX_POINT('',#15117);
#4877=VERTEX_POINT('',#15119);
#4878=VERTEX_POINT('',#15121);
#4879=VERTEX_POINT('',#15123);
#4880=VERTEX_POINT('',#15125);
#4881=VERTEX_POINT('',#15127);
#4882=VERTEX_POINT('',#15148);
#4883=VERTEX_POINT('',#15150);
#4884=VERTEX_POINT('',#15154);
#4885=VERTEX_POINT('',#15156);
#4886=VERTEX_POINT('',#15158);
#4887=VERTEX_POINT('',#15160);
#4888=VERTEX_POINT('',#15162);
#4889=VERTEX_POINT('',#15164);
#4890=VERTEX_POINT('',#15167);
#4891=VERTEX_POINT('',#15169);
#4892=VERTEX_POINT('',#15172);
#4893=VERTEX_POINT('',#15173);
#4894=VERTEX_POINT('',#15175);
#4895=VERTEX_POINT('',#15177);
#4896=VERTEX_POINT('',#15180);
#4897=VERTEX_POINT('',#15181);
#4898=VERTEX_POINT('',#15183);
#4899=VERTEX_POINT('',#15185);
#4900=VERTEX_POINT('',#15188);
#4901=VERTEX_POINT('',#15189);
#4902=VERTEX_POINT('',#15191);
#4903=VERTEX_POINT('',#15193);
#4904=VERTEX_POINT('',#15196);
#4905=VERTEX_POINT('',#15197);
#4906=VERTEX_POINT('',#15199);
#4907=VERTEX_POINT('',#15201);
#4908=VERTEX_POINT('',#15204);
#4909=VERTEX_POINT('',#15205);
#4910=VERTEX_POINT('',#15207);
#4911=VERTEX_POINT('',#15209);
#4912=VERTEX_POINT('',#15212);
#4913=VERTEX_POINT('',#15213);
#4914=VERTEX_POINT('',#15215);
#4915=VERTEX_POINT('',#15217);
#4916=VERTEX_POINT('',#15220);
#4917=VERTEX_POINT('',#15221);
#4918=VERTEX_POINT('',#15223);
#4919=VERTEX_POINT('',#15225);
#4920=VERTEX_POINT('',#15228);
#4921=VERTEX_POINT('',#15229);
#4922=VERTEX_POINT('',#15231);
#4923=VERTEX_POINT('',#15233);
#4924=VERTEX_POINT('',#15236);
#4925=VERTEX_POINT('',#15237);
#4926=VERTEX_POINT('',#15239);
#4927=VERTEX_POINT('',#15241);
#4928=VERTEX_POINT('',#15244);
#4929=VERTEX_POINT('',#15245);
#4930=VERTEX_POINT('',#15247);
#4931=VERTEX_POINT('',#15249);
#4932=VERTEX_POINT('',#15252);
#4933=VERTEX_POINT('',#15253);
#4934=VERTEX_POINT('',#15255);
#4935=VERTEX_POINT('',#15257);
#4936=VERTEX_POINT('',#15260);
#4937=VERTEX_POINT('',#15261);
#4938=VERTEX_POINT('',#15263);
#4939=VERTEX_POINT('',#15265);
#4940=VERTEX_POINT('',#15268);
#4941=VERTEX_POINT('',#15269);
#4942=VERTEX_POINT('',#15271);
#4943=VERTEX_POINT('',#15273);
#4944=VERTEX_POINT('',#15276);
#4945=VERTEX_POINT('',#15277);
#4946=VERTEX_POINT('',#15279);
#4947=VERTEX_POINT('',#15281);
#4948=VERTEX_POINT('',#15284);
#4949=VERTEX_POINT('',#15285);
#4950=VERTEX_POINT('',#15287);
#4951=VERTEX_POINT('',#15289);
#4952=VERTEX_POINT('',#15292);
#4953=VERTEX_POINT('',#15293);
#4954=VERTEX_POINT('',#15295);
#4955=VERTEX_POINT('',#15297);
#4956=VERTEX_POINT('',#15300);
#4957=VERTEX_POINT('',#15301);
#4958=VERTEX_POINT('',#15303);
#4959=VERTEX_POINT('',#15305);
#4960=VERTEX_POINT('',#15308);
#4961=VERTEX_POINT('',#15309);
#4962=VERTEX_POINT('',#15311);
#4963=VERTEX_POINT('',#15313);
#4964=VERTEX_POINT('',#15316);
#4965=VERTEX_POINT('',#15317);
#4966=VERTEX_POINT('',#15319);
#4967=VERTEX_POINT('',#15321);
#4968=VERTEX_POINT('',#15324);
#4969=VERTEX_POINT('',#15325);
#4970=VERTEX_POINT('',#15327);
#4971=VERTEX_POINT('',#15329);
#4972=VERTEX_POINT('',#15332);
#4973=VERTEX_POINT('',#15333);
#4974=VERTEX_POINT('',#15335);
#4975=VERTEX_POINT('',#15337);
#4976=VERTEX_POINT('',#15340);
#4977=VERTEX_POINT('',#15341);
#4978=VERTEX_POINT('',#15343);
#4979=VERTEX_POINT('',#15345);
#4980=VERTEX_POINT('',#15348);
#4981=VERTEX_POINT('',#15349);
#4982=VERTEX_POINT('',#15351);
#4983=VERTEX_POINT('',#15353);
#4984=VERTEX_POINT('',#15356);
#4985=VERTEX_POINT('',#15357);
#4986=VERTEX_POINT('',#15359);
#4987=VERTEX_POINT('',#15361);
#4988=VERTEX_POINT('',#15364);
#4989=VERTEX_POINT('',#15365);
#4990=VERTEX_POINT('',#15367);
#4991=VERTEX_POINT('',#15369);
#4992=VERTEX_POINT('',#15372);
#4993=VERTEX_POINT('',#15373);
#4994=VERTEX_POINT('',#15375);
#4995=VERTEX_POINT('',#15377);
#4996=VERTEX_POINT('',#15380);
#4997=VERTEX_POINT('',#15381);
#4998=VERTEX_POINT('',#15383);
#4999=VERTEX_POINT('',#15385);
#5000=VERTEX_POINT('',#15388);
#5001=VERTEX_POINT('',#15389);
#5002=VERTEX_POINT('',#15391);
#5003=VERTEX_POINT('',#15393);
#5004=VERTEX_POINT('',#15396);
#5005=VERTEX_POINT('',#15397);
#5006=VERTEX_POINT('',#15399);
#5007=VERTEX_POINT('',#15401);
#5008=VERTEX_POINT('',#15404);
#5009=VERTEX_POINT('',#15405);
#5010=VERTEX_POINT('',#15407);
#5011=VERTEX_POINT('',#15409);
#5012=VERTEX_POINT('',#15412);
#5013=VERTEX_POINT('',#15413);
#5014=VERTEX_POINT('',#15415);
#5015=VERTEX_POINT('',#15417);
#5016=VERTEX_POINT('',#15420);
#5017=VERTEX_POINT('',#15421);
#5018=VERTEX_POINT('',#15423);
#5019=VERTEX_POINT('',#15425);
#5020=VERTEX_POINT('',#15428);
#5021=VERTEX_POINT('',#15429);
#5022=VERTEX_POINT('',#15431);
#5023=VERTEX_POINT('',#15433);
#5024=VERTEX_POINT('',#15436);
#5025=VERTEX_POINT('',#15437);
#5026=VERTEX_POINT('',#15439);
#5027=VERTEX_POINT('',#15441);
#5028=VERTEX_POINT('',#15444);
#5029=VERTEX_POINT('',#15445);
#5030=VERTEX_POINT('',#15447);
#5031=VERTEX_POINT('',#15449);
#5032=VERTEX_POINT('',#15452);
#5033=VERTEX_POINT('',#15453);
#5034=VERTEX_POINT('',#15455);
#5035=VERTEX_POINT('',#15457);
#5036=VERTEX_POINT('',#15460);
#5037=VERTEX_POINT('',#15461);
#5038=VERTEX_POINT('',#15463);
#5039=VERTEX_POINT('',#15465);
#5040=VERTEX_POINT('',#15468);
#5041=VERTEX_POINT('',#15469);
#5042=VERTEX_POINT('',#15471);
#5043=VERTEX_POINT('',#15473);
#5044=VERTEX_POINT('',#15476);
#5045=VERTEX_POINT('',#15477);
#5046=VERTEX_POINT('',#15479);
#5047=VERTEX_POINT('',#15481);
#5048=VERTEX_POINT('',#15487);
#5049=VERTEX_POINT('',#15489);
#5050=VERTEX_POINT('',#15493);
#5051=VERTEX_POINT('',#15495);
#5052=VERTEX_POINT('',#15504);
#5053=VERTEX_POINT('',#15506);
#5054=VERTEX_POINT('',#15510);
#5055=VERTEX_POINT('',#15512);
#5056=VERTEX_POINT('',#15521);
#5057=VERTEX_POINT('',#15523);
#5058=VERTEX_POINT('',#15527);
#5059=VERTEX_POINT('',#15529);
#5060=VERTEX_POINT('',#15538);
#5061=VERTEX_POINT('',#15540);
#5062=VERTEX_POINT('',#15544);
#5063=VERTEX_POINT('',#15546);
#5064=VERTEX_POINT('',#15555);
#5065=VERTEX_POINT('',#15557);
#5066=VERTEX_POINT('',#15561);
#5067=VERTEX_POINT('',#15563);
#5068=VERTEX_POINT('',#15572);
#5069=VERTEX_POINT('',#15574);
#5070=VERTEX_POINT('',#15578);
#5071=VERTEX_POINT('',#15580);
#5072=VERTEX_POINT('',#15589);
#5073=VERTEX_POINT('',#15591);
#5074=VERTEX_POINT('',#15595);
#5075=VERTEX_POINT('',#15597);
#5076=VERTEX_POINT('',#15606);
#5077=VERTEX_POINT('',#15608);
#5078=VERTEX_POINT('',#15612);
#5079=VERTEX_POINT('',#15614);
#5080=VERTEX_POINT('',#15623);
#5081=VERTEX_POINT('',#15625);
#5082=VERTEX_POINT('',#15629);
#5083=VERTEX_POINT('',#15631);
#5084=VERTEX_POINT('',#15640);
#5085=VERTEX_POINT('',#15642);
#5086=VERTEX_POINT('',#15646);
#5087=VERTEX_POINT('',#15648);
#5088=VERTEX_POINT('',#15657);
#5089=VERTEX_POINT('',#15659);
#5090=VERTEX_POINT('',#15663);
#5091=VERTEX_POINT('',#15665);
#5092=VERTEX_POINT('',#15674);
#5093=VERTEX_POINT('',#15676);
#5094=VERTEX_POINT('',#15680);
#5095=VERTEX_POINT('',#15682);
#5096=VERTEX_POINT('',#15691);
#5097=VERTEX_POINT('',#15693);
#5098=VERTEX_POINT('',#15697);
#5099=VERTEX_POINT('',#15699);
#5100=VERTEX_POINT('',#15708);
#5101=VERTEX_POINT('',#15710);
#5102=VERTEX_POINT('',#15714);
#5103=VERTEX_POINT('',#15716);
#5104=VERTEX_POINT('',#15725);
#5105=VERTEX_POINT('',#15727);
#5106=VERTEX_POINT('',#15731);
#5107=VERTEX_POINT('',#15733);
#5108=VERTEX_POINT('',#15742);
#5109=VERTEX_POINT('',#15744);
#5110=VERTEX_POINT('',#15748);
#5111=VERTEX_POINT('',#15750);
#5112=VERTEX_POINT('',#15759);
#5113=VERTEX_POINT('',#15761);
#5114=VERTEX_POINT('',#15765);
#5115=VERTEX_POINT('',#15767);
#5116=VERTEX_POINT('',#15776);
#5117=VERTEX_POINT('',#15778);
#5118=VERTEX_POINT('',#15782);
#5119=VERTEX_POINT('',#15784);
#5120=VERTEX_POINT('',#15793);
#5121=VERTEX_POINT('',#15795);
#5122=VERTEX_POINT('',#15799);
#5123=VERTEX_POINT('',#15801);
#5124=VERTEX_POINT('',#15810);
#5125=VERTEX_POINT('',#15812);
#5126=VERTEX_POINT('',#15816);
#5127=VERTEX_POINT('',#15818);
#5128=VERTEX_POINT('',#15827);
#5129=VERTEX_POINT('',#15829);
#5130=VERTEX_POINT('',#15833);
#5131=VERTEX_POINT('',#15835);
#5132=VERTEX_POINT('',#15844);
#5133=VERTEX_POINT('',#15846);
#5134=VERTEX_POINT('',#15850);
#5135=VERTEX_POINT('',#15852);
#5136=VERTEX_POINT('',#15861);
#5137=VERTEX_POINT('',#15863);
#5138=VERTEX_POINT('',#15867);
#5139=VERTEX_POINT('',#15869);
#5140=VERTEX_POINT('',#15878);
#5141=VERTEX_POINT('',#15880);
#5142=VERTEX_POINT('',#15884);
#5143=VERTEX_POINT('',#15886);
#5144=VERTEX_POINT('',#15895);
#5145=VERTEX_POINT('',#15897);
#5146=VERTEX_POINT('',#15901);
#5147=VERTEX_POINT('',#15903);
#5148=VERTEX_POINT('',#15912);
#5149=VERTEX_POINT('',#15914);
#5150=VERTEX_POINT('',#15918);
#5151=VERTEX_POINT('',#15920);
#5152=VERTEX_POINT('',#15929);
#5153=VERTEX_POINT('',#15931);
#5154=VERTEX_POINT('',#15935);
#5155=VERTEX_POINT('',#15937);
#5156=VERTEX_POINT('',#15946);
#5157=VERTEX_POINT('',#15948);
#5158=VERTEX_POINT('',#15952);
#5159=VERTEX_POINT('',#15954);
#5160=VERTEX_POINT('',#15963);
#5161=VERTEX_POINT('',#15965);
#5162=VERTEX_POINT('',#15969);
#5163=VERTEX_POINT('',#15971);
#5164=VERTEX_POINT('',#15980);
#5165=VERTEX_POINT('',#15982);
#5166=VERTEX_POINT('',#15986);
#5167=VERTEX_POINT('',#15988);
#5168=VERTEX_POINT('',#15997);
#5169=VERTEX_POINT('',#15999);
#5170=VERTEX_POINT('',#16003);
#5171=VERTEX_POINT('',#16005);
#5172=VERTEX_POINT('',#16014);
#5173=VERTEX_POINT('',#16016);
#5174=VERTEX_POINT('',#16020);
#5175=VERTEX_POINT('',#16022);
#5176=VERTEX_POINT('',#16031);
#5177=VERTEX_POINT('',#16033);
#5178=VERTEX_POINT('',#16037);
#5179=VERTEX_POINT('',#16039);
#5180=VERTEX_POINT('',#16048);
#5181=VERTEX_POINT('',#16050);
#5182=VERTEX_POINT('',#16054);
#5183=VERTEX_POINT('',#16056);
#5184=VERTEX_POINT('',#16065);
#5185=VERTEX_POINT('',#16067);
#5186=VERTEX_POINT('',#16071);
#5187=VERTEX_POINT('',#16073);
#5188=VERTEX_POINT('',#16082);
#5189=VERTEX_POINT('',#16084);
#5190=VERTEX_POINT('',#16088);
#5191=VERTEX_POINT('',#16090);
#5192=VERTEX_POINT('',#16099);
#5193=VERTEX_POINT('',#16101);
#5194=VERTEX_POINT('',#16105);
#5195=VERTEX_POINT('',#16107);
#5196=VERTEX_POINT('',#16116);
#5197=VERTEX_POINT('',#16118);
#5198=VERTEX_POINT('',#16122);
#5199=VERTEX_POINT('',#16124);
#5200=VERTEX_POINT('',#16133);
#5201=VERTEX_POINT('',#16135);
#5202=VERTEX_POINT('',#16139);
#5203=VERTEX_POINT('',#16141);
#5204=VERTEX_POINT('',#16150);
#5205=VERTEX_POINT('',#16152);
#5206=VERTEX_POINT('',#16156);
#5207=VERTEX_POINT('',#16158);
#5208=VERTEX_POINT('',#16168);
#5209=VERTEX_POINT('',#16170);
#5210=VERTEX_POINT('',#16174);
#5211=VERTEX_POINT('',#16176);
#5212=VERTEX_POINT('',#16180);
#5213=VERTEX_POINT('',#16181);
#5214=VERTEX_POINT('',#16183);
#5215=VERTEX_POINT('',#16185);
#5216=VERTEX_POINT('',#16187);
#5217=VERTEX_POINT('',#16189);
#5218=VERTEX_POINT('',#16191);
#5219=VERTEX_POINT('',#16193);
#5220=VERTEX_POINT('',#16195);
#5221=VERTEX_POINT('',#16197);
#5222=VERTEX_POINT('',#16199);
#5223=VERTEX_POINT('',#16201);
#5224=VERTEX_POINT('',#16203);
#5225=VERTEX_POINT('',#16205);
#5226=VERTEX_POINT('',#16209);
#5227=VERTEX_POINT('',#16210);
#5228=VERTEX_POINT('',#16212);
#5229=VERTEX_POINT('',#16214);
#5230=VERTEX_POINT('',#16216);
#5231=VERTEX_POINT('',#16218);
#5232=VERTEX_POINT('',#16220);
#5233=VERTEX_POINT('',#16222);
#5234=VERTEX_POINT('',#16224);
#5235=VERTEX_POINT('',#16226);
#5236=VERTEX_POINT('',#16228);
#5237=VERTEX_POINT('',#16230);
#5238=VERTEX_POINT('',#16232);
#5239=VERTEX_POINT('',#16234);
#5240=VERTEX_POINT('',#16267);
#5241=VERTEX_POINT('',#16269);
#5242=VERTEX_POINT('',#16273);
#5243=VERTEX_POINT('',#16274);
#5244=VERTEX_POINT('',#16279);
#5245=VERTEX_POINT('',#16283);
#5246=VERTEX_POINT('',#16285);
#5247=VERTEX_POINT('',#16292);
#5248=VERTEX_POINT('',#16294);
#5249=VERTEX_POINT('',#16298);
#5250=VERTEX_POINT('',#16300);
#5251=VERTEX_POINT('',#16308);
#5252=VERTEX_POINT('',#16310);
#5253=VERTEX_POINT('',#16314);
#5254=VERTEX_POINT('',#16315);
#5255=VERTEX_POINT('',#16317);
#5256=VERTEX_POINT('',#16319);
#5257=VERTEX_POINT('',#16321);
#5258=VERTEX_POINT('',#16323);
#5259=VERTEX_POINT('',#16327);
#5260=VERTEX_POINT('',#16328);
#5261=VERTEX_POINT('',#16330);
#5262=VERTEX_POINT('',#16332);
#5263=VERTEX_POINT('',#16334);
#5264=VERTEX_POINT('',#16336);
#5265=VERTEX_POINT('',#16353);
#5266=VERTEX_POINT('',#16355);
#5267=VERTEX_POINT('',#16359);
#5268=VERTEX_POINT('',#16361);
#5269=VERTEX_POINT('',#16365);
#5270=VERTEX_POINT('',#16366);
#5271=VERTEX_POINT('',#16368);
#5272=VERTEX_POINT('',#16370);
#5273=VERTEX_POINT('',#16372);
#5274=VERTEX_POINT('',#16374);
#5275=VERTEX_POINT('',#16380);
#5276=VERTEX_POINT('',#16382);
#5277=VERTEX_POINT('',#16386);
#5278=VERTEX_POINT('',#16390);
#5279=VERTEX_POINT('',#16394);
#5280=VERTEX_POINT('',#16398);
#5281=VERTEX_POINT('',#16406);
#5282=VERTEX_POINT('',#16408);
#5283=VERTEX_POINT('',#16412);
#5284=VERTEX_POINT('',#16413);
#5285=VERTEX_POINT('',#16415);
#5286=VERTEX_POINT('',#16417);
#5287=VERTEX_POINT('',#16421);
#5288=VERTEX_POINT('',#16423);
#5289=VERTEX_POINT('',#16427);
#5290=VERTEX_POINT('',#16429);
#5291=VERTEX_POINT('',#16433);
#5292=VERTEX_POINT('',#16435);
#5293=VERTEX_POINT('',#16439);
#5294=VERTEX_POINT('',#16441);
#5295=VERTEX_POINT('',#16452);
#5296=VERTEX_POINT('',#16454);
#5297=VERTEX_POINT('',#16458);
#5298=VERTEX_POINT('',#16460);
#5299=VERTEX_POINT('',#16464);
#5300=VERTEX_POINT('',#16465);
#5301=VERTEX_POINT('',#16467);
#5302=VERTEX_POINT('',#16469);
#5303=VERTEX_POINT('',#16471);
#5304=VERTEX_POINT('',#16473);
#5305=VERTEX_POINT('',#16479);
#5306=VERTEX_POINT('',#16481);
#5307=VERTEX_POINT('',#16485);
#5308=VERTEX_POINT('',#16489);
#5309=VERTEX_POINT('',#16493);
#5310=VERTEX_POINT('',#16497);
#5311=EDGE_CURVE('',#4455,#4455,#4232,.T.);
#5312=EDGE_CURVE('',#4455,#4456,#2136,.T.);
#5313=EDGE_CURVE('',#4456,#4456,#4233,.T.);
#5314=EDGE_CURVE('',#4457,#4457,#4234,.T.);
#5315=EDGE_CURVE('',#4457,#4458,#2137,.T.);
#5316=EDGE_CURVE('',#4458,#4458,#4235,.T.);
#5317=EDGE_CURVE('',#4459,#4460,#2138,.T.);
#5318=EDGE_CURVE('',#4459,#4461,#2139,.T.);
#5319=EDGE_CURVE('',#4461,#4462,#2140,.T.);
#5320=EDGE_CURVE('',#4463,#4462,#2141,.T.);
#5321=EDGE_CURVE('',#4464,#4463,#2142,.T.);
#5322=EDGE_CURVE('',#4465,#4464,#2143,.T.);
#5323=EDGE_CURVE('',#4465,#4466,#2144,.T.);
#5324=EDGE_CURVE('',#4467,#4466,#2145,.T.);
#5325=EDGE_CURVE('',#4468,#4467,#2146,.T.);
#5326=EDGE_CURVE('',#4469,#4468,#2147,.T.);
#5327=EDGE_CURVE('',#4469,#4470,#2148,.T.);
#5328=EDGE_CURVE('',#4471,#4470,#2149,.T.);
#5329=EDGE_CURVE('',#4472,#4471,#2150,.T.);
#5330=EDGE_CURVE('',#4473,#4472,#2151,.T.);
#5331=EDGE_CURVE('',#4473,#4474,#2152,.T.);
#5332=EDGE_CURVE('',#4474,#4475,#2153,.T.);
#5333=EDGE_CURVE('',#4475,#4476,#2154,.T.);
#5334=EDGE_CURVE('',#4477,#4476,#2155,.T.);
#5335=EDGE_CURVE('',#4478,#4477,#2156,.T.);
#5336=EDGE_CURVE('',#4479,#4478,#2157,.T.);
#5337=EDGE_CURVE('',#4479,#4480,#2158,.T.);
#5338=EDGE_CURVE('',#4481,#4480,#2159,.T.);
#5339=EDGE_CURVE('',#4482,#4481,#2160,.T.);
#5340=EDGE_CURVE('',#4483,#4482,#2161,.T.);
#5341=EDGE_CURVE('',#4483,#4484,#2162,.T.);
#5342=EDGE_CURVE('',#4485,#4484,#2163,.T.);
#5343=EDGE_CURVE('',#4486,#4485,#2164,.T.);
#5344=EDGE_CURVE('',#4487,#4486,#2165,.T.);
#5345=EDGE_CURVE('',#4487,#4488,#2166,.T.);
#5346=EDGE_CURVE('',#4488,#4489,#2167,.T.);
#5347=EDGE_CURVE('',#4490,#4489,#2168,.T.);
#5348=EDGE_CURVE('',#4490,#4460,#2169,.T.);
#5349=EDGE_CURVE('',#4491,#4492,#2170,.T.);
#5350=EDGE_CURVE('',#4491,#4493,#2171,.T.);
#5351=EDGE_CURVE('',#4493,#4494,#2172,.T.);
#5352=EDGE_CURVE('',#4492,#4494,#2173,.T.);
#5353=EDGE_CURVE('',#4495,#4496,#2174,.T.);
#5354=EDGE_CURVE('',#4497,#4495,#2175,.T.);
#5355=EDGE_CURVE('',#4497,#4498,#2176,.T.);
#5356=EDGE_CURVE('',#4498,#4496,#2177,.T.);
#5357=EDGE_CURVE('',#4480,#4499,#2178,.T.);
#5358=EDGE_CURVE('',#4500,#4479,#2179,.T.);
#5359=EDGE_CURVE('',#4500,#4499,#2180,.T.);
#5360=EDGE_CURVE('',#4501,#4483,#2181,.T.);
#5361=EDGE_CURVE('',#4501,#4502,#2182,.T.);
#5362=EDGE_CURVE('',#4484,#4502,#2183,.T.);
#5363=EDGE_CURVE('',#4503,#4487,#2184,.T.);
#5364=EDGE_CURVE('',#4503,#4504,#2185,.T.);
#5365=EDGE_CURVE('',#4488,#4504,#2186,.T.);
#5366=EDGE_CURVE('',#4476,#4505,#2187,.T.);
#5367=EDGE_CURVE('',#4475,#4506,#2188,.T.);
#5368=EDGE_CURVE('',#4506,#4505,#2189,.T.);
#5369=EDGE_CURVE('',#4507,#4473,#2190,.T.);
#5370=EDGE_CURVE('',#4507,#4508,#2191,.T.);
#5371=EDGE_CURVE('',#4474,#4508,#2192,.T.);
#5372=EDGE_CURVE('',#4470,#4509,#2193,.T.);
#5373=EDGE_CURVE('',#4510,#4469,#2194,.T.);
#5374=EDGE_CURVE('',#4510,#4509,#2195,.T.);
#5375=EDGE_CURVE('',#4466,#4511,#2196,.T.);
#5376=EDGE_CURVE('',#4512,#4465,#2197,.T.);
#5377=EDGE_CURVE('',#4512,#4511,#2198,.T.);
#5378=EDGE_CURVE('',#4462,#4513,#2199,.T.);
#5379=EDGE_CURVE('',#4461,#4514,#2200,.T.);
#5380=EDGE_CURVE('',#4514,#4513,#2201,.T.);
#5381=EDGE_CURVE('',#4507,#4515,#2202,.T.);
#5382=EDGE_CURVE('',#4515,#4516,#2203,.T.);
#5383=EDGE_CURVE('',#4516,#4509,#2204,.T.);
#5384=EDGE_CURVE('',#4510,#4517,#2205,.T.);
#5385=EDGE_CURVE('',#4517,#4518,#2206,.T.);
#5386=EDGE_CURVE('',#4518,#4511,#2207,.T.);
#5387=EDGE_CURVE('',#4512,#4519,#2208,.T.);
#5388=EDGE_CURVE('',#4519,#4520,#2209,.T.);
#5389=EDGE_CURVE('',#4520,#4513,#2210,.T.);
#5390=EDGE_CURVE('',#4504,#4514,#2211,.T.);
#5391=EDGE_CURVE('',#4503,#4521,#2212,.T.);
#5392=EDGE_CURVE('',#4521,#4522,#2213,.T.);
#5393=EDGE_CURVE('',#4522,#4502,#2214,.T.);
#5394=EDGE_CURVE('',#4501,#4523,#2215,.T.);
#5395=EDGE_CURVE('',#4523,#4524,#2216,.T.);
#5396=EDGE_CURVE('',#4524,#4499,#2217,.T.);
#5397=EDGE_CURVE('',#4500,#4525,#2218,.T.);
#5398=EDGE_CURVE('',#4525,#4526,#2219,.T.);
#5399=EDGE_CURVE('',#4526,#4505,#2220,.T.);
#5400=EDGE_CURVE('',#4508,#4506,#2221,.T.);
#5401=EDGE_CURVE('',#4489,#4459,#4236,.T.);
#5402=EDGE_CURVE('',#4527,#4498,#2222,.T.);
#5403=EDGE_CURVE('',#4528,#4497,#2223,.T.);
#5404=EDGE_CURVE('',#4528,#4527,#2224,.T.);
#5405=EDGE_CURVE('',#4496,#4529,#2225,.T.);
#5406=EDGE_CURVE('',#4530,#4529,#2226,.T.);
#5407=EDGE_CURVE('',#4495,#4530,#2227,.T.);
#5408=EDGE_CURVE('',#4529,#4531,#2228,.T.);
#5409=EDGE_CURVE('',#4532,#4531,#2229,.T.);
#5410=EDGE_CURVE('',#4530,#4532,#2230,.T.);
#5411=EDGE_CURVE('',#4531,#4527,#2231,.T.);
#5412=EDGE_CURVE('',#4532,#4528,#2232,.T.);
#5413=EDGE_CURVE('',#4494,#4533,#2233,.T.);
#5414=EDGE_CURVE('',#4534,#4533,#2234,.T.);
#5415=EDGE_CURVE('',#4492,#4534,#2235,.T.);
#5416=EDGE_CURVE('',#4533,#4535,#2236,.T.);
#5417=EDGE_CURVE('',#4536,#4535,#2237,.T.);
#5418=EDGE_CURVE('',#4534,#4536,#2238,.T.);
#5419=EDGE_CURVE('',#4535,#4537,#2239,.T.);
#5420=EDGE_CURVE('',#4538,#4537,#2240,.T.);
#5421=EDGE_CURVE('',#4536,#4538,#2241,.T.);
#5422=EDGE_CURVE('',#4537,#4493,#2242,.T.);
#5423=EDGE_CURVE('',#4538,#4491,#2243,.T.);
#5424=EDGE_CURVE('',#4464,#4519,#2244,.T.);
#5425=EDGE_CURVE('',#4463,#4520,#2245,.T.);
#5426=EDGE_CURVE('',#4477,#4526,#2246,.T.);
#5427=EDGE_CURVE('',#4478,#4525,#2247,.T.);
#5428=EDGE_CURVE('',#4485,#4522,#2248,.T.);
#5429=EDGE_CURVE('',#4486,#4521,#2249,.T.);
#5430=EDGE_CURVE('',#4468,#4517,#2250,.T.);
#5431=EDGE_CURVE('',#4467,#4518,#2251,.T.);
#5432=EDGE_CURVE('',#4481,#4524,#2252,.T.);
#5433=EDGE_CURVE('',#4482,#4523,#2253,.T.);
#5434=EDGE_CURVE('',#4472,#4515,#2254,.T.);
#5435=EDGE_CURVE('',#4471,#4516,#2255,.T.);
#5436=EDGE_CURVE('',#4460,#4490,#4237,.T.);
#5437=EDGE_CURVE('',#4539,#4540,#4238,.T.);
#5438=EDGE_CURVE('',#4540,#4541,#2256,.T.);
#5439=EDGE_CURVE('',#4542,#4541,#4239,.T.);
#5440=EDGE_CURVE('',#4542,#4539,#2257,.T.);
#5441=EDGE_CURVE('',#4543,#4543,#4240,.T.);
#5442=EDGE_CURVE('',#4543,#4544,#2258,.T.);
#5443=EDGE_CURVE('',#4544,#4544,#4241,.T.);
#5444=EDGE_CURVE('',#4545,#4545,#4242,.T.);
#5445=EDGE_CURVE('',#4545,#4546,#2259,.T.);
#5446=EDGE_CURVE('',#4546,#4546,#4243,.T.);
#5447=EDGE_CURVE('',#4547,#4547,#4244,.T.);
#5448=EDGE_CURVE('',#4547,#4548,#2260,.T.);
#5449=EDGE_CURVE('',#4548,#4549,#195,.T.);
#5450=EDGE_CURVE('',#4550,#4549,#4245,.T.);
#5451=EDGE_CURVE('',#4550,#4548,#196,.T.);
#5452=EDGE_CURVE('',#4551,#4551,#4246,.T.);
#5453=EDGE_CURVE('',#4551,#4552,#2261,.T.);
#5454=EDGE_CURVE('',#4552,#4553,#197,.T.);
#5455=EDGE_CURVE('',#4554,#4553,#4247,.T.);
#5456=EDGE_CURVE('',#4554,#4552,#198,.T.);
#5457=EDGE_CURVE('',#4555,#4555,#4248,.T.);
#5458=EDGE_CURVE('',#4555,#4556,#2262,.T.);
#5459=EDGE_CURVE('',#4556,#4557,#199,.T.);
#5460=EDGE_CURVE('',#4558,#4557,#4249,.T.);
#5461=EDGE_CURVE('',#4558,#4556,#200,.T.);
#5462=EDGE_CURVE('',#4541,#4542,#2263,.T.);
#5463=EDGE_CURVE('',#4540,#4559,#2264,.T.);
#5464=EDGE_CURVE('',#4559,#4560,#2265,.T.);
#5465=EDGE_CURVE('',#4561,#4560,#2266,.T.);
#5466=EDGE_CURVE('',#4562,#4561,#2267,.T.);
#5467=EDGE_CURVE('',#4562,#4539,#2268,.T.);
#5468=EDGE_CURVE('',#4563,#4564,#2269,.T.);
#5469=EDGE_CURVE('',#4563,#4565,#2270,.T.);
#5470=EDGE_CURVE('',#4565,#4566,#2271,.T.);
#5471=EDGE_CURVE('',#4564,#4566,#2272,.T.);
#5472=EDGE_CURVE('',#4567,#4568,#2273,.T.);
#5473=EDGE_CURVE('',#4569,#4567,#2274,.T.);
#5474=EDGE_CURVE('',#4569,#4570,#2275,.T.);
#5475=EDGE_CURVE('',#4570,#4568,#2276,.T.);
#5476=EDGE_CURVE('',#4571,#4572,#2277,.T.);
#5477=EDGE_CURVE('',#4573,#4572,#2278,.T.);
#5478=EDGE_CURVE('',#4574,#4573,#2279,.T.);
#5479=EDGE_CURVE('',#4574,#4571,#2280,.T.);
#5480=EDGE_CURVE('',#4557,#4558,#2281,.T.);
#5481=EDGE_CURVE('',#4549,#4550,#2282,.T.);
#5482=EDGE_CURVE('',#4553,#4554,#2283,.T.);
#5483=EDGE_CURVE('',#4560,#4575,#2284,.T.);
#5484=EDGE_CURVE('',#4576,#4575,#2285,.T.);
#5485=EDGE_CURVE('',#4561,#4576,#2286,.T.);
#5486=EDGE_CURVE('',#4575,#4577,#2287,.T.);
#5487=EDGE_CURVE('',#4578,#4577,#2288,.T.);
#5488=EDGE_CURVE('',#4576,#4578,#2289,.T.);
#5489=EDGE_CURVE('',#4577,#4579,#2290,.T.);
#5490=EDGE_CURVE('',#4580,#4579,#2291,.T.);
#5491=EDGE_CURVE('',#4578,#4580,#2292,.T.);
#5492=EDGE_CURVE('',#4579,#4581,#2293,.T.);
#5493=EDGE_CURVE('',#4582,#4581,#2294,.T.);
#5494=EDGE_CURVE('',#4580,#4582,#2295,.T.);
#5495=EDGE_CURVE('',#4581,#4583,#2296,.T.);
#5496=EDGE_CURVE('',#4584,#4583,#2297,.T.);
#5497=EDGE_CURVE('',#4582,#4584,#2298,.T.);
#5498=EDGE_CURVE('',#4583,#4571,#2299,.T.);
#5499=EDGE_CURVE('',#4584,#4574,#2300,.T.);
#5500=EDGE_CURVE('',#4572,#4585,#2301,.T.);
#5501=EDGE_CURVE('',#4586,#4585,#2302,.T.);
#5502=EDGE_CURVE('',#4573,#4586,#2303,.T.);
#5503=EDGE_CURVE('',#4585,#4587,#2304,.T.);
#5504=EDGE_CURVE('',#4588,#4587,#2305,.T.);
#5505=EDGE_CURVE('',#4586,#4588,#2306,.T.);
#5506=EDGE_CURVE('',#4587,#4589,#2307,.T.);
#5507=EDGE_CURVE('',#4590,#4589,#2308,.T.);
#5508=EDGE_CURVE('',#4588,#4590,#2309,.T.);
#5509=EDGE_CURVE('',#4590,#4562,#2310,.T.);
#5510=EDGE_CURVE('',#4589,#4559,#2311,.T.);
#5511=EDGE_CURVE('',#4566,#4591,#2312,.T.);
#5512=EDGE_CURVE('',#4592,#4591,#2313,.T.);
#5513=EDGE_CURVE('',#4564,#4592,#2314,.T.);
#5514=EDGE_CURVE('',#4591,#4593,#2315,.T.);
#5515=EDGE_CURVE('',#4594,#4593,#2316,.T.);
#5516=EDGE_CURVE('',#4592,#4594,#2317,.T.);
#5517=EDGE_CURVE('',#4593,#4595,#2318,.T.);
#5518=EDGE_CURVE('',#4596,#4595,#2319,.T.);
#5519=EDGE_CURVE('',#4594,#4596,#2320,.T.);
#5520=EDGE_CURVE('',#4595,#4565,#2321,.T.);
#5521=EDGE_CURVE('',#4596,#4563,#2322,.T.);
#5522=EDGE_CURVE('',#4597,#4570,#2323,.T.);
#5523=EDGE_CURVE('',#4598,#4569,#2324,.T.);
#5524=EDGE_CURVE('',#4598,#4597,#2325,.T.);
#5525=EDGE_CURVE('',#4568,#4599,#2326,.T.);
#5526=EDGE_CURVE('',#4600,#4599,#2327,.T.);
#5527=EDGE_CURVE('',#4567,#4600,#2328,.T.);
#5528=EDGE_CURVE('',#4599,#4601,#2329,.T.);
#5529=EDGE_CURVE('',#4602,#4601,#2330,.T.);
#5530=EDGE_CURVE('',#4600,#4602,#2331,.T.);
#5531=EDGE_CURVE('',#4601,#4597,#2332,.T.);
#5532=EDGE_CURVE('',#4602,#4598,#2333,.T.);
#5533=EDGE_CURVE('',#4603,#4603,#4250,.T.);
#5534=EDGE_CURVE('',#4603,#4604,#2334,.T.);
#5535=EDGE_CURVE('',#4605,#4604,#4251,.T.);
#5536=EDGE_CURVE('',#4605,#4606,#201,.T.);
#5537=EDGE_CURVE('',#4604,#4606,#4252,.T.);
#5538=EDGE_CURVE('',#4607,#4607,#4253,.T.);
#5539=EDGE_CURVE('',#4607,#4608,#2335,.T.);
#5540=EDGE_CURVE('',#4609,#4608,#4254,.T.);
#5541=EDGE_CURVE('',#4609,#4610,#202,.T.);
#5542=EDGE_CURVE('',#4608,#4610,#4255,.T.);
#5543=EDGE_CURVE('',#4611,#4611,#4256,.T.);
#5544=EDGE_CURVE('',#4611,#4612,#2336,.T.);
#5545=EDGE_CURVE('',#4613,#4612,#4257,.T.);
#5546=EDGE_CURVE('',#4613,#4614,#203,.T.);
#5547=EDGE_CURVE('',#4612,#4614,#4258,.T.);
#5548=EDGE_CURVE('',#4615,#4615,#4259,.T.);
#5549=EDGE_CURVE('',#4615,#4616,#2337,.T.);
#5550=EDGE_CURVE('',#4616,#4616,#4260,.T.);
#5551=EDGE_CURVE('',#4617,#4617,#4261,.T.);
#5552=EDGE_CURVE('',#4617,#4618,#2338,.T.);
#5553=EDGE_CURVE('',#4618,#4618,#4262,.T.);
#5554=EDGE_CURVE('',#4619,#4619,#4263,.T.);
#5555=EDGE_CURVE('',#4619,#4620,#2339,.T.);
#5556=EDGE_CURVE('',#4620,#4620,#4264,.T.);
#5557=EDGE_CURVE('',#4621,#4622,#2340,.T.);
#5558=EDGE_CURVE('',#4623,#4621,#2341,.T.);
#5559=EDGE_CURVE('',#4623,#4624,#2342,.T.);
#5560=EDGE_CURVE('',#4624,#4625,#2343,.T.);
#5561=EDGE_CURVE('',#4626,#4625,#2344,.T.);
#5562=EDGE_CURVE('',#4626,#4627,#2345,.T.);
#5563=EDGE_CURVE('',#4627,#4628,#2346,.T.);
#5564=EDGE_CURVE('',#4628,#4629,#2347,.T.);
#5565=EDGE_CURVE('',#4630,#4629,#2348,.T.);
#5566=EDGE_CURVE('',#4630,#4631,#2349,.T.);
#5567=EDGE_CURVE('',#4631,#4632,#2350,.T.);
#5568=EDGE_CURVE('',#4632,#4622,#2351,.T.);
#5569=EDGE_CURVE('',#4633,#4634,#2352,.T.);
#5570=EDGE_CURVE('',#4635,#4633,#2353,.T.);
#5571=EDGE_CURVE('',#4635,#4636,#2354,.T.);
#5572=EDGE_CURVE('',#4637,#4636,#2355,.T.);
#5573=EDGE_CURVE('',#4638,#4637,#2356,.T.);
#5574=EDGE_CURVE('',#4639,#4638,#2357,.T.);
#5575=EDGE_CURVE('',#4640,#4639,#2358,.T.);
#5576=EDGE_CURVE('',#4641,#4640,#2359,.T.);
#5577=EDGE_CURVE('',#4642,#4641,#2360,.T.);
#5578=EDGE_CURVE('',#4643,#4642,#2361,.T.);
#5579=EDGE_CURVE('',#4644,#4643,#2362,.T.);
#5580=EDGE_CURVE('',#4634,#4644,#2363,.T.);
#5581=EDGE_CURVE('',#4645,#4646,#2364,.T.);
#5582=EDGE_CURVE('',#4646,#4647,#2365,.T.);
#5583=EDGE_CURVE('',#4648,#4647,#2366,.T.);
#5584=EDGE_CURVE('',#4649,#4648,#2367,.T.);
#5585=EDGE_CURVE('',#4650,#4649,#2368,.T.);
#5586=EDGE_CURVE('',#4651,#4650,#2369,.T.);
#5587=EDGE_CURVE('',#4652,#4651,#2370,.T.);
#5588=EDGE_CURVE('',#4653,#4652,#2371,.T.);
#5589=EDGE_CURVE('',#4654,#4653,#2372,.T.);
#5590=EDGE_CURVE('',#4655,#4654,#2373,.T.);
#5591=EDGE_CURVE('',#4656,#4655,#2374,.T.);
#5592=EDGE_CURVE('',#4656,#4645,#2375,.T.);
#5593=EDGE_CURVE('',#4647,#4657,#2376,.T.);
#5594=EDGE_CURVE('',#4657,#4658,#2377,.T.);
#5595=EDGE_CURVE('',#4658,#4656,#2378,.T.);
#5596=EDGE_CURVE('',#4659,#4655,#2379,.T.);
#5597=EDGE_CURVE('',#4660,#4659,#2380,.T.);
#5598=EDGE_CURVE('',#4648,#4660,#2381,.T.);
#5599=EDGE_CURVE('',#4633,#4661,#2382,.T.);
#5600=EDGE_CURVE('',#4661,#4662,#2383,.T.);
#5601=EDGE_CURVE('',#4635,#4662,#2384,.T.);
#5602=EDGE_CURVE('',#4663,#4664,#2385,.T.);
#5603=EDGE_CURVE('',#4664,#4643,#2386,.T.);
#5604=EDGE_CURVE('',#4642,#4663,#2387,.T.);
#5605=EDGE_CURVE('',#4665,#4666,#2388,.T.);
#5606=EDGE_CURVE('',#4665,#4637,#2389,.T.);
#5607=EDGE_CURVE('',#4666,#4636,#2390,.T.);
#5608=EDGE_CURVE('',#4640,#4667,#2391,.T.);
#5609=EDGE_CURVE('',#4668,#4667,#2392,.T.);
#5610=EDGE_CURVE('',#4668,#4641,#2393,.T.);
#5611=EDGE_CURVE('',#4661,#4669,#2394,.T.);
#5612=EDGE_CURVE('',#4669,#4670,#2395,.T.);
#5613=EDGE_CURVE('',#4662,#4670,#2396,.T.);
#5614=EDGE_CURVE('',#4671,#4672,#2397,.T.);
#5615=EDGE_CURVE('',#4672,#4664,#2398,.T.);
#5616=EDGE_CURVE('',#4663,#4671,#2399,.T.);
#5617=EDGE_CURVE('',#4673,#4674,#2400,.T.);
#5618=EDGE_CURVE('',#4673,#4675,#2401,.T.);
#5619=EDGE_CURVE('',#4675,#4676,#2402,.T.);
#5620=EDGE_CURVE('',#4674,#4676,#2403,.T.);
#5621=EDGE_CURVE('',#4677,#4678,#2404,.T.);
#5622=EDGE_CURVE('',#4678,#4679,#2405,.T.);
#5623=EDGE_CURVE('',#4680,#4679,#2406,.T.);
#5624=EDGE_CURVE('',#4680,#4677,#2407,.T.);
#5625=EDGE_CURVE('',#4681,#4682,#2408,.T.);
#5626=EDGE_CURVE('',#4681,#4665,#2409,.T.);
#5627=EDGE_CURVE('',#4682,#4666,#2410,.T.);
#5628=EDGE_CURVE('',#4667,#4683,#2411,.T.);
#5629=EDGE_CURVE('',#4684,#4683,#2412,.T.);
#5630=EDGE_CURVE('',#4684,#4668,#2413,.T.);
#5631=EDGE_CURVE('',#4685,#4652,#2414,.T.);
#5632=EDGE_CURVE('',#4686,#4685,#2415,.T.);
#5633=EDGE_CURVE('',#4686,#4653,#2416,.T.);
#5634=EDGE_CURVE('',#4614,#4613,#2417,.T.);
#5635=EDGE_CURVE('',#4606,#4605,#2418,.T.);
#5636=EDGE_CURVE('',#4610,#4609,#2419,.T.);
#5637=EDGE_CURVE('',#4687,#4688,#2420,.T.);
#5638=EDGE_CURVE('',#4687,#4689,#2421,.T.);
#5639=EDGE_CURVE('',#4626,#4689,#2422,.T.);
#5640=EDGE_CURVE('',#4625,#4659,#2423,.T.);
#5641=EDGE_CURVE('',#4688,#4654,#2424,.T.);
#5642=EDGE_CURVE('',#4688,#4686,#2425,.T.);
#5643=EDGE_CURVE('',#4690,#4651,#2426,.T.);
#5644=EDGE_CURVE('',#4685,#4690,#2427,.T.);
#5645=EDGE_CURVE('',#4691,#4650,#2428,.T.);
#5646=EDGE_CURVE('',#4690,#4691,#2429,.T.);
#5647=EDGE_CURVE('',#4692,#4649,#2430,.T.);
#5648=EDGE_CURVE('',#4691,#4692,#2431,.T.);
#5649=EDGE_CURVE('',#4632,#4660,#2432,.T.);
#5650=EDGE_CURVE('',#4631,#4693,#2433,.T.);
#5651=EDGE_CURVE('',#4693,#4694,#2434,.T.);
#5652=EDGE_CURVE('',#4692,#4694,#2435,.T.);
#5653=EDGE_CURVE('',#4694,#4687,#2436,.T.);
#5654=EDGE_CURVE('',#4695,#4624,#2437,.T.);
#5655=EDGE_CURVE('',#4696,#4695,#2438,.T.);
#5656=EDGE_CURVE('',#4697,#4696,#2439,.T.);
#5657=EDGE_CURVE('',#4698,#4697,#2440,.T.);
#5658=EDGE_CURVE('',#4622,#4698,#2441,.T.);
#5659=EDGE_CURVE('',#4689,#4693,#2442,.T.);
#5660=EDGE_CURVE('',#4630,#4699,#2443,.T.);
#5661=EDGE_CURVE('',#4699,#4700,#2444,.T.);
#5662=EDGE_CURVE('',#4700,#4701,#2445,.T.);
#5663=EDGE_CURVE('',#4701,#4702,#2446,.T.);
#5664=EDGE_CURVE('',#4702,#4627,#2447,.T.);
#5665=EDGE_CURVE('',#4629,#4703,#2448,.T.);
#5666=EDGE_CURVE('',#4699,#4703,#2449,.T.);
#5667=EDGE_CURVE('',#4703,#4704,#2450,.T.);
#5668=EDGE_CURVE('',#4700,#4704,#2451,.T.);
#5669=EDGE_CURVE('',#4704,#4705,#2452,.T.);
#5670=EDGE_CURVE('',#4701,#4705,#2453,.T.);
#5671=EDGE_CURVE('',#4705,#4706,#2454,.T.);
#5672=EDGE_CURVE('',#4702,#4706,#2455,.T.);
#5673=EDGE_CURVE('',#4706,#4628,#2456,.T.);
#5674=EDGE_CURVE('',#4707,#4698,#2457,.T.);
#5675=EDGE_CURVE('',#4621,#4707,#2458,.T.);
#5676=EDGE_CURVE('',#4708,#4697,#2459,.T.);
#5677=EDGE_CURVE('',#4707,#4708,#2460,.T.);
#5678=EDGE_CURVE('',#4709,#4696,#2461,.T.);
#5679=EDGE_CURVE('',#4708,#4709,#2462,.T.);
#5680=EDGE_CURVE('',#4710,#4695,#2463,.T.);
#5681=EDGE_CURVE('',#4709,#4710,#2464,.T.);
#5682=EDGE_CURVE('',#4710,#4623,#2465,.T.);
#5683=EDGE_CURVE('',#4677,#4684,#2466,.T.);
#5684=EDGE_CURVE('',#4671,#4680,#2467,.T.);
#5685=EDGE_CURVE('',#4670,#4674,#2468,.T.);
#5686=EDGE_CURVE('',#4676,#4682,#2469,.T.);
#5687=EDGE_CURVE('',#4673,#4658,#2470,.T.);
#5688=EDGE_CURVE('',#4634,#4669,#2471,.T.);
#5689=EDGE_CURVE('',#4644,#4672,#2472,.T.);
#5690=EDGE_CURVE('',#4679,#4711,#2473,.T.);
#5691=EDGE_CURVE('',#4645,#4711,#2474,.T.);
#5692=EDGE_CURVE('',#4638,#4681,#2475,.T.);
#5693=EDGE_CURVE('',#4675,#4657,#2476,.T.);
#5694=EDGE_CURVE('',#4712,#4646,#2477,.T.);
#5695=EDGE_CURVE('',#4678,#4712,#2478,.T.);
#5696=EDGE_CURVE('',#4639,#4683,#2479,.T.);
#5697=EDGE_CURVE('',#4711,#4712,#2480,.T.);
#5698=EDGE_CURVE('',#4713,#4713,#4265,.T.);
#5699=EDGE_CURVE('',#4713,#4714,#2481,.T.);
#5700=EDGE_CURVE('',#4714,#4714,#4266,.T.);
#5701=EDGE_CURVE('',#4715,#4715,#4267,.T.);
#5702=EDGE_CURVE('',#4715,#4716,#2482,.T.);
#5703=EDGE_CURVE('',#4716,#4716,#4268,.T.);
#5704=EDGE_CURVE('',#4717,#4717,#4269,.T.);
#5705=EDGE_CURVE('',#4717,#4718,#2483,.T.);
#5706=EDGE_CURVE('',#4718,#4718,#4270,.T.);
#5707=EDGE_CURVE('',#4719,#4719,#4271,.T.);
#5708=EDGE_CURVE('',#4719,#4720,#2484,.T.);
#5709=EDGE_CURVE('',#4720,#4720,#4272,.T.);
#5710=EDGE_CURVE('',#4721,#4721,#4273,.T.);
#5711=EDGE_CURVE('',#4721,#4722,#2485,.T.);
#5712=EDGE_CURVE('',#4722,#4722,#4274,.T.);
#5713=EDGE_CURVE('',#4723,#4724,#2486,.T.);
#5714=EDGE_CURVE('',#4725,#4723,#2487,.T.);
#5715=EDGE_CURVE('',#4725,#4726,#2488,.T.);
#5716=EDGE_CURVE('',#4726,#4724,#2489,.T.);
#5717=EDGE_CURVE('',#4727,#4728,#2490,.T.);
#5718=EDGE_CURVE('',#4727,#4729,#2491,.T.);
#5719=EDGE_CURVE('',#4730,#4729,#2492,.T.);
#5720=EDGE_CURVE('',#4728,#4730,#2493,.T.);
#5721=EDGE_CURVE('',#4729,#4731,#2494,.T.);
#5722=EDGE_CURVE('',#4732,#4731,#2495,.T.);
#5723=EDGE_CURVE('',#4730,#4732,#2496,.T.);
#5724=EDGE_CURVE('',#4731,#4733,#2497,.T.);
#5725=EDGE_CURVE('',#4734,#4733,#2498,.T.);
#5726=EDGE_CURVE('',#4732,#4734,#2499,.T.);
#5727=EDGE_CURVE('',#4733,#4735,#2500,.T.);
#5728=EDGE_CURVE('',#4736,#4735,#2501,.T.);
#5729=EDGE_CURVE('',#4734,#4736,#2502,.T.);
#5730=EDGE_CURVE('',#4735,#4737,#2503,.T.);
#5731=EDGE_CURVE('',#4738,#4737,#2504,.T.);
#5732=EDGE_CURVE('',#4736,#4738,#2505,.T.);
#5733=EDGE_CURVE('',#4737,#4726,#2506,.T.);
#5734=EDGE_CURVE('',#4738,#4725,#2507,.T.);
#5735=EDGE_CURVE('',#4723,#4739,#2508,.T.);
#5736=EDGE_CURVE('',#4739,#4740,#2509,.T.);
#5737=EDGE_CURVE('',#4728,#4740,#2510,.T.);
#5738=EDGE_CURVE('',#4727,#4741,#2511,.T.);
#5739=EDGE_CURVE('',#4741,#4742,#2512,.T.);
#5740=EDGE_CURVE('',#4724,#4742,#2513,.T.);
#5741=EDGE_CURVE('',#4742,#4739,#2514,.T.);
#5742=EDGE_CURVE('',#4740,#4741,#2515,.T.);
#5743=EDGE_CURVE('',#4743,#4744,#2516,.T.);
#5744=EDGE_CURVE('',#4745,#4744,#2517,.T.);
#5745=EDGE_CURVE('',#4746,#4745,#2518,.T.);
#5746=EDGE_CURVE('',#4746,#4743,#2519,.T.);
#5747=EDGE_CURVE('',#4744,#4747,#2520,.T.);
#5748=EDGE_CURVE('',#4748,#4747,#2521,.T.);
#5749=EDGE_CURVE('',#4745,#4748,#2522,.T.);
#5750=EDGE_CURVE('',#4747,#4749,#2523,.T.);
#5751=EDGE_CURVE('',#4750,#4749,#2524,.T.);
#5752=EDGE_CURVE('',#4748,#4750,#2525,.T.);
#5753=EDGE_CURVE('',#4749,#4743,#2526,.T.);
#5754=EDGE_CURVE('',#4750,#4746,#2527,.T.);
#5755=EDGE_CURVE('',#4751,#4752,#2528,.T.);
#5756=EDGE_CURVE('',#4753,#4752,#2529,.T.);
#5757=EDGE_CURVE('',#4754,#4753,#2530,.T.);
#5758=EDGE_CURVE('',#4754,#4751,#2531,.T.);
#5759=EDGE_CURVE('',#4752,#4755,#2532,.T.);
#5760=EDGE_CURVE('',#4756,#4755,#2533,.T.);
#5761=EDGE_CURVE('',#4753,#4756,#2534,.T.);
#5762=EDGE_CURVE('',#4755,#4757,#2535,.T.);
#5763=EDGE_CURVE('',#4758,#4757,#2536,.T.);
#5764=EDGE_CURVE('',#4756,#4758,#2537,.T.);
#5765=EDGE_CURVE('',#4757,#4751,#2538,.T.);
#5766=EDGE_CURVE('',#4758,#4754,#2539,.T.);
#5767=EDGE_CURVE('',#4759,#4759,#4275,.T.);
#5768=EDGE_CURVE('',#4759,#4760,#2540,.T.);
#5769=EDGE_CURVE('',#4760,#4760,#4276,.T.);
#5770=EDGE_CURVE('',#4761,#4761,#4277,.T.);
#5771=EDGE_CURVE('',#4761,#4762,#2541,.T.);
#5772=EDGE_CURVE('',#4762,#4762,#4278,.T.);
#5773=EDGE_CURVE('',#4763,#4763,#4279,.T.);
#5774=EDGE_CURVE('',#4763,#4764,#2542,.T.);
#5775=EDGE_CURVE('',#4764,#4764,#4280,.T.);
#5776=EDGE_CURVE('',#4765,#4765,#4281,.T.);
#5777=EDGE_CURVE('',#4765,#4766,#2543,.T.);
#5778=EDGE_CURVE('',#4766,#4766,#4282,.T.);
#5779=EDGE_CURVE('',#4767,#4768,#2544,.T.);
#5780=EDGE_CURVE('',#4769,#4768,#2545,.T.);
#5781=EDGE_CURVE('',#4770,#4769,#2546,.T.);
#5782=EDGE_CURVE('',#4770,#4767,#2547,.T.);
#5783=EDGE_CURVE('',#4768,#4771,#2548,.T.);
#5784=EDGE_CURVE('',#4772,#4771,#2549,.T.);
#5785=EDGE_CURVE('',#4769,#4772,#2550,.T.);
#5786=EDGE_CURVE('',#4771,#4773,#2551,.T.);
#5787=EDGE_CURVE('',#4774,#4773,#2552,.T.);
#5788=EDGE_CURVE('',#4772,#4774,#2553,.T.);
#5789=EDGE_CURVE('',#4773,#4767,#2554,.T.);
#5790=EDGE_CURVE('',#4774,#4770,#2555,.T.);
#5791=EDGE_CURVE('',#4775,#4775,#4283,.T.);
#5792=EDGE_CURVE('',#4775,#4776,#2556,.T.);
#5793=EDGE_CURVE('',#4776,#4776,#4284,.T.);
#5794=EDGE_CURVE('',#4777,#4777,#4285,.T.);
#5795=EDGE_CURVE('',#4777,#4778,#2557,.T.);
#5796=EDGE_CURVE('',#4778,#4778,#4286,.T.);
#5797=EDGE_CURVE('',#4779,#4779,#4287,.T.);
#5798=EDGE_CURVE('',#4779,#4780,#2558,.T.);
#5799=EDGE_CURVE('',#4780,#4780,#4288,.T.);
#5800=EDGE_CURVE('',#4781,#4781,#4289,.T.);
#5801=EDGE_CURVE('',#4781,#4782,#2559,.T.);
#5802=EDGE_CURVE('',#4782,#4782,#4290,.T.);
#5803=EDGE_CURVE('',#4783,#4783,#4291,.T.);
#5804=EDGE_CURVE('',#4783,#4784,#2560,.T.);
#5805=EDGE_CURVE('',#4784,#4784,#4292,.T.);
#5806=EDGE_CURVE('',#4785,#4785,#4293,.T.);
#5807=EDGE_CURVE('',#4785,#4786,#2561,.T.);
#5808=EDGE_CURVE('',#4786,#4786,#4294,.T.);
#5809=EDGE_CURVE('',#4787,#4787,#4295,.T.);
#5810=EDGE_CURVE('',#4787,#4788,#2562,.T.);
#5811=EDGE_CURVE('',#4788,#4788,#4296,.T.);
#5812=EDGE_CURVE('',#4789,#4789,#4297,.T.);
#5813=EDGE_CURVE('',#4789,#4790,#2563,.T.);
#5814=EDGE_CURVE('',#4790,#4790,#4298,.T.);
#5815=EDGE_CURVE('',#4791,#4791,#4299,.T.);
#5816=EDGE_CURVE('',#4791,#4792,#2564,.T.);
#5817=EDGE_CURVE('',#4792,#4792,#4300,.T.);
#5818=EDGE_CURVE('',#4793,#4793,#4301,.T.);
#5819=EDGE_CURVE('',#4793,#4794,#2565,.T.);
#5820=EDGE_CURVE('',#4794,#4794,#4302,.T.);
#5821=EDGE_CURVE('',#4795,#4795,#4303,.T.);
#5822=EDGE_CURVE('',#4795,#4796,#2566,.T.);
#5823=EDGE_CURVE('',#4796,#4797,#189,.T.);
#5824=EDGE_CURVE('',#4797,#4796,#190,.T.);
#5825=EDGE_CURVE('',#4798,#4799,#191,.T.);
#5826=EDGE_CURVE('',#4799,#4800,#2567,.T.);
#5827=EDGE_CURVE('',#4800,#4800,#4304,.T.);
#5828=EDGE_CURVE('',#4799,#4798,#192,.T.);
#5829=EDGE_CURVE('',#4801,#4801,#4305,.T.);
#5830=EDGE_CURVE('',#4801,#4802,#2568,.T.);
#5831=EDGE_CURVE('',#4802,#4802,#4306,.T.);
#5832=EDGE_CURVE('',#4803,#4803,#4307,.T.);
#5833=EDGE_CURVE('',#4803,#4804,#2569,.T.);
#5834=EDGE_CURVE('',#4804,#4804,#4308,.T.);
#5835=EDGE_CURVE('',#4805,#4806,#4309,.T.);
#5836=EDGE_CURVE('',#4807,#4805,#2570,.T.);
#5837=EDGE_CURVE('',#4807,#4808,#4310,.T.);
#5838=EDGE_CURVE('',#4809,#4808,#2571,.T.);
#5839=EDGE_CURVE('',#4810,#4809,#4311,.T.);
#5840=EDGE_CURVE('',#4810,#4799,#2572,.T.);
#5841=EDGE_CURVE('',#4798,#4811,#2573,.T.);
#5842=EDGE_CURVE('',#4811,#4811,#4312,.T.);
#5843=EDGE_CURVE('',#4812,#4810,#4313,.T.);
#5844=EDGE_CURVE('',#4813,#4812,#2574,.T.);
#5845=EDGE_CURVE('',#4813,#4814,#4314,.T.);
#5846=EDGE_CURVE('',#4806,#4814,#2575,.T.);
#5847=EDGE_CURVE('',#4805,#4806,#2576,.T.);
#5848=EDGE_CURVE('',#4812,#4809,#2577,.T.);
#5849=EDGE_CURVE('',#4814,#4807,#2578,.T.);
#5850=EDGE_CURVE('',#4808,#4813,#2579,.T.);
#5851=EDGE_CURVE('',#4815,#4815,#4315,.T.);
#5852=EDGE_CURVE('',#4815,#4816,#2580,.T.);
#5853=EDGE_CURVE('',#4816,#4816,#4316,.T.);
#5854=EDGE_CURVE('',#4817,#4818,#2581,.T.);
#5855=EDGE_CURVE('',#4818,#4819,#2582,.T.);
#5856=EDGE_CURVE('',#4819,#4820,#2583,.T.);
#5857=EDGE_CURVE('',#4820,#4817,#2584,.T.);
#5858=EDGE_CURVE('',#4821,#4822,#2585,.T.);
#5859=EDGE_CURVE('',#4823,#4821,#2586,.T.);
#5860=EDGE_CURVE('',#4824,#4823,#2587,.T.);
#5861=EDGE_CURVE('',#4822,#4824,#2588,.T.);
#5862=EDGE_CURVE('',#4818,#4822,#2589,.T.);
#5863=EDGE_CURVE('',#4817,#4821,#2590,.T.);
#5864=EDGE_CURVE('',#4819,#4824,#2591,.T.);
#5865=EDGE_CURVE('',#4820,#4823,#2592,.T.);
#5866=EDGE_CURVE('',#4825,#4825,#4317,.T.);
#5867=EDGE_CURVE('',#4825,#4826,#2593,.T.);
#5868=EDGE_CURVE('',#4826,#4826,#4318,.T.);
#5869=EDGE_CURVE('',#4827,#4828,#2594,.T.);
#5870=EDGE_CURVE('',#4828,#4829,#2595,.T.);
#5871=EDGE_CURVE('',#4829,#4830,#2596,.T.);
#5872=EDGE_CURVE('',#4830,#4827,#2597,.T.);
#5873=EDGE_CURVE('',#4831,#4832,#2598,.T.);
#5874=EDGE_CURVE('',#4833,#4831,#2599,.T.);
#5875=EDGE_CURVE('',#4834,#4833,#2600,.T.);
#5876=EDGE_CURVE('',#4832,#4834,#2601,.T.);
#5877=EDGE_CURVE('',#4828,#4832,#2602,.T.);
#5878=EDGE_CURVE('',#4827,#4831,#2603,.T.);
#5879=EDGE_CURVE('',#4829,#4834,#2604,.T.);
#5880=EDGE_CURVE('',#4830,#4833,#2605,.T.);
#5881=EDGE_CURVE('',#4835,#4835,#4319,.T.);
#5882=EDGE_CURVE('',#4835,#4836,#2606,.T.);
#5883=EDGE_CURVE('',#4836,#4836,#4320,.T.);
#5884=EDGE_CURVE('',#4837,#4837,#4321,.T.);
#5885=EDGE_CURVE('',#4837,#4838,#193,.T.);
#5886=EDGE_CURVE('',#4838,#4838,#4322,.T.);
#5887=EDGE_CURVE('',#4838,#4837,#194,.T.);
#5888=EDGE_CURVE('',#4839,#4839,#4323,.T.);
#5889=EDGE_CURVE('',#4839,#4840,#2607,.T.);
#5890=EDGE_CURVE('',#4840,#4840,#4324,.T.);
#5891=EDGE_CURVE('',#4841,#4841,#4325,.T.);
#5892=EDGE_CURVE('',#4841,#4837,#2608,.T.);
#5893=EDGE_CURVE('',#4842,#4842,#4326,.T.);
#5894=EDGE_CURVE('',#4842,#4843,#2609,.T.);
#5895=EDGE_CURVE('',#4843,#4843,#4327,.T.);
#5896=EDGE_CURVE('',#4844,#4844,#4328,.T.);
#5897=EDGE_CURVE('',#4844,#4845,#2610,.T.);
#5898=EDGE_CURVE('',#4845,#4845,#4329,.T.);
#5899=EDGE_CURVE('',#4846,#4846,#4330,.T.);
#5900=EDGE_CURVE('',#4846,#4847,#2611,.T.);
#5901=EDGE_CURVE('',#4847,#4847,#4331,.T.);
#5902=EDGE_CURVE('',#4848,#4848,#4332,.T.);
#5903=EDGE_CURVE('',#4848,#4849,#2612,.T.);
#5904=EDGE_CURVE('',#4849,#4849,#4333,.T.);
#5905=EDGE_CURVE('',#4850,#4850,#4334,.T.);
#5906=EDGE_CURVE('',#4850,#4851,#2613,.T.);
#5907=EDGE_CURVE('',#4851,#4851,#4335,.T.);
#5908=EDGE_CURVE('',#4852,#4853,#2614,.T.);
#5909=EDGE_CURVE('',#4854,#4853,#2615,.T.);
#5910=EDGE_CURVE('',#4855,#4854,#2616,.T.);
#5911=EDGE_CURVE('',#4855,#4852,#2617,.T.);
#5912=EDGE_CURVE('',#4853,#4856,#2618,.T.);
#5913=EDGE_CURVE('',#4857,#4856,#2619,.T.);
#5914=EDGE_CURVE('',#4854,#4857,#2620,.T.);
#5915=EDGE_CURVE('',#4856,#4858,#2621,.T.);
#5916=EDGE_CURVE('',#4859,#4858,#2622,.T.);
#5917=EDGE_CURVE('',#4857,#4859,#2623,.T.);
#5918=EDGE_CURVE('',#4858,#4852,#2624,.T.);
#5919=EDGE_CURVE('',#4859,#4855,#2625,.T.);
#5920=EDGE_CURVE('',#4860,#4860,#4336,.T.);
#5921=EDGE_CURVE('',#4860,#4861,#2626,.T.);
#5922=EDGE_CURVE('',#4861,#4861,#4337,.T.);
#5923=EDGE_CURVE('',#4862,#4862,#4338,.T.);
#5924=EDGE_CURVE('',#4862,#4863,#2627,.T.);
#5925=EDGE_CURVE('',#4863,#4863,#4339,.T.);
#5926=EDGE_CURVE('',#4864,#4864,#4340,.T.);
#5927=EDGE_CURVE('',#4864,#4865,#2628,.T.);
#5928=EDGE_CURVE('',#4865,#4865,#4341,.T.);
#5929=EDGE_CURVE('',#4866,#4867,#2629,.T.);
#5930=EDGE_CURVE('',#4867,#4868,#2630,.T.);
#5931=EDGE_CURVE('',#4868,#4869,#2631,.T.);
#5932=EDGE_CURVE('',#4869,#4870,#2632,.T.);
#5933=EDGE_CURVE('',#4870,#4871,#2633,.T.);
#5934=EDGE_CURVE('',#4871,#4872,#2634,.T.);
#5935=EDGE_CURVE('',#4872,#4873,#2635,.T.);
#5936=EDGE_CURVE('',#4873,#4866,#2636,.T.);
#5937=EDGE_CURVE('',#4874,#4875,#2637,.T.);
#5938=EDGE_CURVE('',#4876,#4874,#2638,.T.);
#5939=EDGE_CURVE('',#4877,#4876,#2639,.T.);
#5940=EDGE_CURVE('',#4878,#4877,#2640,.T.);
#5941=EDGE_CURVE('',#4879,#4878,#2641,.T.);
#5942=EDGE_CURVE('',#4880,#4879,#2642,.T.);
#5943=EDGE_CURVE('',#4881,#4880,#2643,.T.);
#5944=EDGE_CURVE('',#4875,#4881,#2644,.T.);
#5945=EDGE_CURVE('',#4867,#4875,#2645,.T.);
#5946=EDGE_CURVE('',#4866,#4874,#2646,.T.);
#5947=EDGE_CURVE('',#4868,#4881,#2647,.T.);
#5948=EDGE_CURVE('',#4869,#4880,#2648,.T.);
#5949=EDGE_CURVE('',#4870,#4879,#2649,.T.);
#5950=EDGE_CURVE('',#4871,#4878,#2650,.T.);
#5951=EDGE_CURVE('',#4872,#4877,#2651,.T.);
#5952=EDGE_CURVE('',#4873,#4876,#2652,.T.);
#5953=EDGE_CURVE('',#4882,#4882,#4342,.T.);
#5954=EDGE_CURVE('',#4882,#4883,#2653,.T.);
#5955=EDGE_CURVE('',#4883,#4883,#4343,.T.);
#5956=EDGE_CURVE('',#4884,#4884,#4344,.T.);
#5957=EDGE_CURVE('',#4884,#4885,#2654,.T.);
#5958=EDGE_CURVE('',#4886,#4885,#4345,.T.);
#5959=EDGE_CURVE('',#4887,#4886,#2655,.T.);
#5960=EDGE_CURVE('',#4887,#4888,#4346,.T.);
#5961=EDGE_CURVE('',#4888,#4889,#2656,.T.);
#5962=EDGE_CURVE('',#4889,#4889,#4347,.T.);
#5963=EDGE_CURVE('',#4888,#4890,#4348,.T.);
#5964=EDGE_CURVE('',#4891,#4890,#2657,.T.);
#5965=EDGE_CURVE('',#4885,#4891,#4349,.T.);
#5966=EDGE_CURVE('',#4892,#4893,#4350,.T.);
#5967=EDGE_CURVE('',#4894,#4893,#2658,.T.);
#5968=EDGE_CURVE('',#4895,#4894,#4351,.T.);
#5969=EDGE_CURVE('',#4892,#4895,#2659,.T.);
#5970=EDGE_CURVE('',#4896,#4897,#2660,.T.);
#5971=EDGE_CURVE('',#4896,#4898,#4352,.T.);
#5972=EDGE_CURVE('',#4899,#4898,#2661,.T.);
#5973=EDGE_CURVE('',#4897,#4899,#4353,.T.);
#5974=EDGE_CURVE('',#4900,#4901,#2662,.T.);
#5975=EDGE_CURVE('',#4900,#4902,#4354,.T.);
#5976=EDGE_CURVE('',#4903,#4902,#2663,.T.);
#5977=EDGE_CURVE('',#4901,#4903,#4355,.T.);
#5978=EDGE_CURVE('',#4904,#4905,#2664,.T.);
#5979=EDGE_CURVE('',#4904,#4906,#4356,.T.);
#5980=EDGE_CURVE('',#4907,#4906,#2665,.T.);
#5981=EDGE_CURVE('',#4905,#4907,#4357,.T.);
#5982=EDGE_CURVE('',#4908,#4909,#2666,.T.);
#5983=EDGE_CURVE('',#4908,#4910,#4358,.T.);
#5984=EDGE_CURVE('',#4911,#4910,#2667,.T.);
#5985=EDGE_CURVE('',#4909,#4911,#4359,.T.);
#5986=EDGE_CURVE('',#4912,#4913,#2668,.T.);
#5987=EDGE_CURVE('',#4912,#4914,#4360,.T.);
#5988=EDGE_CURVE('',#4915,#4914,#2669,.T.);
#5989=EDGE_CURVE('',#4913,#4915,#4361,.T.);
#5990=EDGE_CURVE('',#4916,#4917,#2670,.T.);
#5991=EDGE_CURVE('',#4916,#4918,#4362,.T.);
#5992=EDGE_CURVE('',#4919,#4918,#2671,.T.);
#5993=EDGE_CURVE('',#4917,#4919,#4363,.T.);
#5994=EDGE_CURVE('',#4920,#4921,#2672,.T.);
#5995=EDGE_CURVE('',#4920,#4922,#4364,.T.);
#5996=EDGE_CURVE('',#4923,#4922,#2673,.T.);
#5997=EDGE_CURVE('',#4921,#4923,#4365,.T.);
#5998=EDGE_CURVE('',#4924,#4925,#2674,.T.);
#5999=EDGE_CURVE('',#4924,#4926,#4366,.T.);
#6000=EDGE_CURVE('',#4927,#4926,#2675,.T.);
#6001=EDGE_CURVE('',#4925,#4927,#4367,.T.);
#6002=EDGE_CURVE('',#4928,#4929,#2676,.T.);
#6003=EDGE_CURVE('',#4928,#4930,#4368,.T.);
#6004=EDGE_CURVE('',#4931,#4930,#2677,.T.);
#6005=EDGE_CURVE('',#4929,#4931,#4369,.T.);
#6006=EDGE_CURVE('',#4932,#4933,#2678,.T.);
#6007=EDGE_CURVE('',#4932,#4934,#4370,.T.);
#6008=EDGE_CURVE('',#4935,#4934,#2679,.T.);
#6009=EDGE_CURVE('',#4933,#4935,#4371,.T.);
#6010=EDGE_CURVE('',#4936,#4937,#2680,.T.);
#6011=EDGE_CURVE('',#4936,#4938,#4372,.T.);
#6012=EDGE_CURVE('',#4939,#4938,#2681,.T.);
#6013=EDGE_CURVE('',#4937,#4939,#4373,.T.);
#6014=EDGE_CURVE('',#4940,#4941,#2682,.T.);
#6015=EDGE_CURVE('',#4940,#4942,#4374,.T.);
#6016=EDGE_CURVE('',#4943,#4942,#2683,.T.);
#6017=EDGE_CURVE('',#4941,#4943,#4375,.T.);
#6018=EDGE_CURVE('',#4944,#4945,#2684,.T.);
#6019=EDGE_CURVE('',#4944,#4946,#4376,.T.);
#6020=EDGE_CURVE('',#4947,#4946,#2685,.T.);
#6021=EDGE_CURVE('',#4945,#4947,#4377,.T.);
#6022=EDGE_CURVE('',#4948,#4949,#2686,.T.);
#6023=EDGE_CURVE('',#4948,#4950,#4378,.T.);
#6024=EDGE_CURVE('',#4951,#4950,#2687,.T.);
#6025=EDGE_CURVE('',#4949,#4951,#4379,.T.);
#6026=EDGE_CURVE('',#4952,#4953,#2688,.T.);
#6027=EDGE_CURVE('',#4952,#4954,#4380,.T.);
#6028=EDGE_CURVE('',#4955,#4954,#2689,.T.);
#6029=EDGE_CURVE('',#4953,#4955,#4381,.T.);
#6030=EDGE_CURVE('',#4956,#4957,#2690,.T.);
#6031=EDGE_CURVE('',#4956,#4958,#4382,.T.);
#6032=EDGE_CURVE('',#4959,#4958,#2691,.T.);
#6033=EDGE_CURVE('',#4957,#4959,#4383,.T.);
#6034=EDGE_CURVE('',#4960,#4961,#2692,.T.);
#6035=EDGE_CURVE('',#4960,#4962,#4384,.T.);
#6036=EDGE_CURVE('',#4963,#4962,#2693,.T.);
#6037=EDGE_CURVE('',#4961,#4963,#4385,.T.);
#6038=EDGE_CURVE('',#4964,#4965,#2694,.T.);
#6039=EDGE_CURVE('',#4964,#4966,#4386,.T.);
#6040=EDGE_CURVE('',#4967,#4966,#2695,.T.);
#6041=EDGE_CURVE('',#4965,#4967,#4387,.T.);
#6042=EDGE_CURVE('',#4968,#4969,#2696,.T.);
#6043=EDGE_CURVE('',#4968,#4970,#4388,.T.);
#6044=EDGE_CURVE('',#4971,#4970,#2697,.T.);
#6045=EDGE_CURVE('',#4969,#4971,#4389,.T.);
#6046=EDGE_CURVE('',#4972,#4973,#2698,.T.);
#6047=EDGE_CURVE('',#4972,#4974,#4390,.T.);
#6048=EDGE_CURVE('',#4975,#4974,#2699,.T.);
#6049=EDGE_CURVE('',#4973,#4975,#4391,.T.);
#6050=EDGE_CURVE('',#4976,#4977,#2700,.T.);
#6051=EDGE_CURVE('',#4976,#4978,#4392,.T.);
#6052=EDGE_CURVE('',#4979,#4978,#2701,.T.);
#6053=EDGE_CURVE('',#4977,#4979,#4393,.T.);
#6054=EDGE_CURVE('',#4980,#4981,#2702,.T.);
#6055=EDGE_CURVE('',#4980,#4982,#4394,.T.);
#6056=EDGE_CURVE('',#4983,#4982,#2703,.T.);
#6057=EDGE_CURVE('',#4981,#4983,#4395,.T.);
#6058=EDGE_CURVE('',#4984,#4985,#2704,.T.);
#6059=EDGE_CURVE('',#4984,#4986,#4396,.T.);
#6060=EDGE_CURVE('',#4987,#4986,#2705,.T.);
#6061=EDGE_CURVE('',#4985,#4987,#4397,.T.);
#6062=EDGE_CURVE('',#4988,#4989,#2706,.T.);
#6063=EDGE_CURVE('',#4988,#4990,#4398,.T.);
#6064=EDGE_CURVE('',#4991,#4990,#2707,.T.);
#6065=EDGE_CURVE('',#4989,#4991,#4399,.T.);
#6066=EDGE_CURVE('',#4992,#4993,#2708,.T.);
#6067=EDGE_CURVE('',#4992,#4994,#4400,.T.);
#6068=EDGE_CURVE('',#4995,#4994,#2709,.T.);
#6069=EDGE_CURVE('',#4993,#4995,#4401,.T.);
#6070=EDGE_CURVE('',#4996,#4997,#2710,.T.);
#6071=EDGE_CURVE('',#4996,#4998,#4402,.T.);
#6072=EDGE_CURVE('',#4999,#4998,#2711,.T.);
#6073=EDGE_CURVE('',#4997,#4999,#4403,.T.);
#6074=EDGE_CURVE('',#5000,#5001,#2712,.T.);
#6075=EDGE_CURVE('',#5000,#5002,#4404,.T.);
#6076=EDGE_CURVE('',#5003,#5002,#2713,.T.);
#6077=EDGE_CURVE('',#5001,#5003,#4405,.T.);
#6078=EDGE_CURVE('',#5004,#5005,#2714,.T.);
#6079=EDGE_CURVE('',#5004,#5006,#4406,.T.);
#6080=EDGE_CURVE('',#5007,#5006,#2715,.T.);
#6081=EDGE_CURVE('',#5005,#5007,#4407,.T.);
#6082=EDGE_CURVE('',#5008,#5009,#2716,.T.);
#6083=EDGE_CURVE('',#5008,#5010,#4408,.T.);
#6084=EDGE_CURVE('',#5011,#5010,#2717,.T.);
#6085=EDGE_CURVE('',#5009,#5011,#4409,.T.);
#6086=EDGE_CURVE('',#5012,#5013,#2718,.T.);
#6087=EDGE_CURVE('',#5012,#5014,#4410,.T.);
#6088=EDGE_CURVE('',#5015,#5014,#2719,.T.);
#6089=EDGE_CURVE('',#5013,#5015,#4411,.T.);
#6090=EDGE_CURVE('',#5016,#5017,#2720,.T.);
#6091=EDGE_CURVE('',#5016,#5018,#4412,.T.);
#6092=EDGE_CURVE('',#5019,#5018,#2721,.T.);
#6093=EDGE_CURVE('',#5017,#5019,#4413,.T.);
#6094=EDGE_CURVE('',#5020,#5021,#2722,.T.);
#6095=EDGE_CURVE('',#5020,#5022,#4414,.T.);
#6096=EDGE_CURVE('',#5023,#5022,#2723,.T.);
#6097=EDGE_CURVE('',#5021,#5023,#4415,.T.);
#6098=EDGE_CURVE('',#5024,#5025,#2724,.T.);
#6099=EDGE_CURVE('',#5024,#5026,#4416,.T.);
#6100=EDGE_CURVE('',#5027,#5026,#2725,.T.);
#6101=EDGE_CURVE('',#5025,#5027,#4417,.T.);
#6102=EDGE_CURVE('',#5028,#5029,#2726,.T.);
#6103=EDGE_CURVE('',#5028,#5030,#4418,.T.);
#6104=EDGE_CURVE('',#5031,#5030,#2727,.T.);
#6105=EDGE_CURVE('',#5029,#5031,#4419,.T.);
#6106=EDGE_CURVE('',#5032,#5033,#2728,.T.);
#6107=EDGE_CURVE('',#5032,#5034,#4420,.T.);
#6108=EDGE_CURVE('',#5035,#5034,#2729,.T.);
#6109=EDGE_CURVE('',#5033,#5035,#4421,.T.);
#6110=EDGE_CURVE('',#5036,#5037,#2730,.T.);
#6111=EDGE_CURVE('',#5036,#5038,#4422,.T.);
#6112=EDGE_CURVE('',#5039,#5038,#2731,.T.);
#6113=EDGE_CURVE('',#5037,#5039,#4423,.T.);
#6114=EDGE_CURVE('',#5040,#5041,#2732,.T.);
#6115=EDGE_CURVE('',#5040,#5042,#4424,.T.);
#6116=EDGE_CURVE('',#5043,#5042,#2733,.T.);
#6117=EDGE_CURVE('',#5041,#5043,#4425,.T.);
#6118=EDGE_CURVE('',#5044,#5045,#2734,.T.);
#6119=EDGE_CURVE('',#5044,#5046,#4426,.T.);
#6120=EDGE_CURVE('',#5047,#5046,#2735,.T.);
#6121=EDGE_CURVE('',#5045,#5047,#4427,.T.);
#6122=EDGE_CURVE('',#5048,#4897,#2736,.T.);
#6123=EDGE_CURVE('',#5049,#5048,#2737,.T.);
#6124=EDGE_CURVE('',#5049,#4896,#2738,.T.);
#6125=EDGE_CURVE('',#4898,#5050,#2739,.T.);
#6126=EDGE_CURVE('',#5050,#5051,#2740,.T.);
#6127=EDGE_CURVE('',#4899,#5051,#2741,.T.);
#6128=EDGE_CURVE('',#5050,#5049,#2742,.T.);
#6129=EDGE_CURVE('',#5051,#5048,#2743,.T.);
#6130=EDGE_CURVE('',#5052,#4901,#2744,.T.);
#6131=EDGE_CURVE('',#5053,#5052,#2745,.T.);
#6132=EDGE_CURVE('',#5053,#4900,#2746,.T.);
#6133=EDGE_CURVE('',#4902,#5054,#2747,.T.);
#6134=EDGE_CURVE('',#5054,#5055,#2748,.T.);
#6135=EDGE_CURVE('',#4903,#5055,#2749,.T.);
#6136=EDGE_CURVE('',#5054,#5053,#2750,.T.);
#6137=EDGE_CURVE('',#5055,#5052,#2751,.T.);
#6138=EDGE_CURVE('',#5056,#4905,#2752,.T.);
#6139=EDGE_CURVE('',#5057,#5056,#2753,.T.);
#6140=EDGE_CURVE('',#5057,#4904,#2754,.T.);
#6141=EDGE_CURVE('',#4906,#5058,#2755,.T.);
#6142=EDGE_CURVE('',#5058,#5059,#2756,.T.);
#6143=EDGE_CURVE('',#4907,#5059,#2757,.T.);
#6144=EDGE_CURVE('',#5058,#5057,#2758,.T.);
#6145=EDGE_CURVE('',#5059,#5056,#2759,.T.);
#6146=EDGE_CURVE('',#5060,#4895,#2760,.T.);
#6147=EDGE_CURVE('',#5061,#5060,#2761,.T.);
#6148=EDGE_CURVE('',#5061,#4892,#2762,.T.);
#6149=EDGE_CURVE('',#4893,#5062,#2763,.T.);
#6150=EDGE_CURVE('',#5062,#5063,#2764,.T.);
#6151=EDGE_CURVE('',#4894,#5063,#2765,.T.);
#6152=EDGE_CURVE('',#5062,#5061,#2766,.T.);
#6153=EDGE_CURVE('',#5063,#5060,#2767,.T.);
#6154=EDGE_CURVE('',#5064,#4973,#2768,.T.);
#6155=EDGE_CURVE('',#5065,#5064,#2769,.T.);
#6156=EDGE_CURVE('',#5065,#4972,#2770,.T.);
#6157=EDGE_CURVE('',#4974,#5066,#2771,.T.);
#6158=EDGE_CURVE('',#5066,#5067,#2772,.T.);
#6159=EDGE_CURVE('',#4975,#5067,#2773,.T.);
#6160=EDGE_CURVE('',#5066,#5065,#2774,.T.);
#6161=EDGE_CURVE('',#5067,#5064,#2775,.T.);
#6162=EDGE_CURVE('',#5068,#4977,#2776,.T.);
#6163=EDGE_CURVE('',#5069,#5068,#2777,.T.);
#6164=EDGE_CURVE('',#5069,#4976,#2778,.T.);
#6165=EDGE_CURVE('',#4978,#5070,#2779,.T.);
#6166=EDGE_CURVE('',#5070,#5071,#2780,.T.);
#6167=EDGE_CURVE('',#4979,#5071,#2781,.T.);
#6168=EDGE_CURVE('',#5070,#5069,#2782,.T.);
#6169=EDGE_CURVE('',#5071,#5068,#2783,.T.);
#6170=EDGE_CURVE('',#5072,#4981,#2784,.T.);
#6171=EDGE_CURVE('',#5073,#5072,#2785,.T.);
#6172=EDGE_CURVE('',#5073,#4980,#2786,.T.);
#6173=EDGE_CURVE('',#4982,#5074,#2787,.T.);
#6174=EDGE_CURVE('',#5074,#5075,#2788,.T.);
#6175=EDGE_CURVE('',#4983,#5075,#2789,.T.);
#6176=EDGE_CURVE('',#5074,#5073,#2790,.T.);
#6177=EDGE_CURVE('',#5075,#5072,#2791,.T.);
#6178=EDGE_CURVE('',#5076,#4886,#2792,.T.);
#6179=EDGE_CURVE('',#5077,#5076,#2793,.T.);
#6180=EDGE_CURVE('',#5077,#4887,#2794,.T.);
#6181=EDGE_CURVE('',#4890,#5078,#2795,.T.);
#6182=EDGE_CURVE('',#5078,#5079,#2796,.T.);
#6183=EDGE_CURVE('',#4891,#5079,#2797,.T.);
#6184=EDGE_CURVE('',#5078,#5077,#2798,.T.);
#6185=EDGE_CURVE('',#5079,#5076,#2799,.T.);
#6186=EDGE_CURVE('',#5080,#4985,#2800,.T.);
#6187=EDGE_CURVE('',#5081,#5080,#2801,.T.);
#6188=EDGE_CURVE('',#5081,#4984,#2802,.T.);
#6189=EDGE_CURVE('',#4986,#5082,#2803,.T.);
#6190=EDGE_CURVE('',#5082,#5083,#2804,.T.);
#6191=EDGE_CURVE('',#4987,#5083,#2805,.T.);
#6192=EDGE_CURVE('',#5082,#5081,#2806,.T.);
#6193=EDGE_CURVE('',#5083,#5080,#2807,.T.);
#6194=EDGE_CURVE('',#5084,#4909,#2808,.T.);
#6195=EDGE_CURVE('',#5085,#5084,#2809,.T.);
#6196=EDGE_CURVE('',#5085,#4908,#2810,.T.);
#6197=EDGE_CURVE('',#4910,#5086,#2811,.T.);
#6198=EDGE_CURVE('',#5086,#5087,#2812,.T.);
#6199=EDGE_CURVE('',#4911,#5087,#2813,.T.);
#6200=EDGE_CURVE('',#5086,#5085,#2814,.T.);
#6201=EDGE_CURVE('',#5087,#5084,#2815,.T.);
#6202=EDGE_CURVE('',#5088,#4913,#2816,.T.);
#6203=EDGE_CURVE('',#5089,#5088,#2817,.T.);
#6204=EDGE_CURVE('',#5089,#4912,#2818,.T.);
#6205=EDGE_CURVE('',#4914,#5090,#2819,.T.);
#6206=EDGE_CURVE('',#5090,#5091,#2820,.T.);
#6207=EDGE_CURVE('',#4915,#5091,#2821,.T.);
#6208=EDGE_CURVE('',#5090,#5089,#2822,.T.);
#6209=EDGE_CURVE('',#5091,#5088,#2823,.T.);
#6210=EDGE_CURVE('',#5092,#4917,#2824,.T.);
#6211=EDGE_CURVE('',#5093,#5092,#2825,.T.);
#6212=EDGE_CURVE('',#5093,#4916,#2826,.T.);
#6213=EDGE_CURVE('',#4918,#5094,#2827,.T.);
#6214=EDGE_CURVE('',#5094,#5095,#2828,.T.);
#6215=EDGE_CURVE('',#4919,#5095,#2829,.T.);
#6216=EDGE_CURVE('',#5094,#5093,#2830,.T.);
#6217=EDGE_CURVE('',#5095,#5092,#2831,.T.);
#6218=EDGE_CURVE('',#5096,#4921,#2832,.T.);
#6219=EDGE_CURVE('',#5097,#5096,#2833,.T.);
#6220=EDGE_CURVE('',#5097,#4920,#2834,.T.);
#6221=EDGE_CURVE('',#4922,#5098,#2835,.T.);
#6222=EDGE_CURVE('',#5098,#5099,#2836,.T.);
#6223=EDGE_CURVE('',#4923,#5099,#2837,.T.);
#6224=EDGE_CURVE('',#5098,#5097,#2838,.T.);
#6225=EDGE_CURVE('',#5099,#5096,#2839,.T.);
#6226=EDGE_CURVE('',#5100,#4925,#2840,.T.);
#6227=EDGE_CURVE('',#5101,#5100,#2841,.T.);
#6228=EDGE_CURVE('',#5101,#4924,#2842,.T.);
#6229=EDGE_CURVE('',#4926,#5102,#2843,.T.);
#6230=EDGE_CURVE('',#5102,#5103,#2844,.T.);
#6231=EDGE_CURVE('',#4927,#5103,#2845,.T.);
#6232=EDGE_CURVE('',#5102,#5101,#2846,.T.);
#6233=EDGE_CURVE('',#5103,#5100,#2847,.T.);
#6234=EDGE_CURVE('',#5104,#4929,#2848,.T.);
#6235=EDGE_CURVE('',#5105,#5104,#2849,.T.);
#6236=EDGE_CURVE('',#5105,#4928,#2850,.T.);
#6237=EDGE_CURVE('',#4930,#5106,#2851,.T.);
#6238=EDGE_CURVE('',#5106,#5107,#2852,.T.);
#6239=EDGE_CURVE('',#4931,#5107,#2853,.T.);
#6240=EDGE_CURVE('',#5106,#5105,#2854,.T.);
#6241=EDGE_CURVE('',#5107,#5104,#2855,.T.);
#6242=EDGE_CURVE('',#5108,#4933,#2856,.T.);
#6243=EDGE_CURVE('',#5109,#5108,#2857,.T.);
#6244=EDGE_CURVE('',#5109,#4932,#2858,.T.);
#6245=EDGE_CURVE('',#4934,#5110,#2859,.T.);
#6246=EDGE_CURVE('',#5110,#5111,#2860,.T.);
#6247=EDGE_CURVE('',#4935,#5111,#2861,.T.);
#6248=EDGE_CURVE('',#5110,#5109,#2862,.T.);
#6249=EDGE_CURVE('',#5111,#5108,#2863,.T.);
#6250=EDGE_CURVE('',#5112,#4937,#2864,.T.);
#6251=EDGE_CURVE('',#5113,#5112,#2865,.T.);
#6252=EDGE_CURVE('',#5113,#4936,#2866,.T.);
#6253=EDGE_CURVE('',#4938,#5114,#2867,.T.);
#6254=EDGE_CURVE('',#5114,#5115,#2868,.T.);
#6255=EDGE_CURVE('',#4939,#5115,#2869,.T.);
#6256=EDGE_CURVE('',#5114,#5113,#2870,.T.);
#6257=EDGE_CURVE('',#5115,#5112,#2871,.T.);
#6258=EDGE_CURVE('',#5116,#4941,#2872,.T.);
#6259=EDGE_CURVE('',#5117,#5116,#2873,.T.);
#6260=EDGE_CURVE('',#5117,#4940,#2874,.T.);
#6261=EDGE_CURVE('',#4942,#5118,#2875,.T.);
#6262=EDGE_CURVE('',#5118,#5119,#2876,.T.);
#6263=EDGE_CURVE('',#4943,#5119,#2877,.T.);
#6264=EDGE_CURVE('',#5118,#5117,#2878,.T.);
#6265=EDGE_CURVE('',#5119,#5116,#2879,.T.);
#6266=EDGE_CURVE('',#5120,#4945,#2880,.T.);
#6267=EDGE_CURVE('',#5121,#5120,#2881,.T.);
#6268=EDGE_CURVE('',#5121,#4944,#2882,.T.);
#6269=EDGE_CURVE('',#4946,#5122,#2883,.T.);
#6270=EDGE_CURVE('',#5122,#5123,#2884,.T.);
#6271=EDGE_CURVE('',#4947,#5123,#2885,.T.);
#6272=EDGE_CURVE('',#5122,#5121,#2886,.T.);
#6273=EDGE_CURVE('',#5123,#5120,#2887,.T.);
#6274=EDGE_CURVE('',#5124,#4949,#2888,.T.);
#6275=EDGE_CURVE('',#5125,#5124,#2889,.T.);
#6276=EDGE_CURVE('',#5125,#4948,#2890,.T.);
#6277=EDGE_CURVE('',#4950,#5126,#2891,.T.);
#6278=EDGE_CURVE('',#5126,#5127,#2892,.T.);
#6279=EDGE_CURVE('',#4951,#5127,#2893,.T.);
#6280=EDGE_CURVE('',#5126,#5125,#2894,.T.);
#6281=EDGE_CURVE('',#5127,#5124,#2895,.T.);
#6282=EDGE_CURVE('',#5128,#4953,#2896,.T.);
#6283=EDGE_CURVE('',#5129,#5128,#2897,.T.);
#6284=EDGE_CURVE('',#5129,#4952,#2898,.T.);
#6285=EDGE_CURVE('',#4954,#5130,#2899,.T.);
#6286=EDGE_CURVE('',#5130,#5131,#2900,.T.);
#6287=EDGE_CURVE('',#4955,#5131,#2901,.T.);
#6288=EDGE_CURVE('',#5130,#5129,#2902,.T.);
#6289=EDGE_CURVE('',#5131,#5128,#2903,.T.);
#6290=EDGE_CURVE('',#5132,#4957,#2904,.T.);
#6291=EDGE_CURVE('',#5133,#5132,#2905,.T.);
#6292=EDGE_CURVE('',#5133,#4956,#2906,.T.);
#6293=EDGE_CURVE('',#4958,#5134,#2907,.T.);
#6294=EDGE_CURVE('',#5134,#5135,#2908,.T.);
#6295=EDGE_CURVE('',#4959,#5135,#2909,.T.);
#6296=EDGE_CURVE('',#5134,#5133,#2910,.T.);
#6297=EDGE_CURVE('',#5135,#5132,#2911,.T.);
#6298=EDGE_CURVE('',#5136,#4961,#2912,.T.);
#6299=EDGE_CURVE('',#5137,#5136,#2913,.T.);
#6300=EDGE_CURVE('',#5137,#4960,#2914,.T.);
#6301=EDGE_CURVE('',#4962,#5138,#2915,.T.);
#6302=EDGE_CURVE('',#5138,#5139,#2916,.T.);
#6303=EDGE_CURVE('',#4963,#5139,#2917,.T.);
#6304=EDGE_CURVE('',#5138,#5137,#2918,.T.);
#6305=EDGE_CURVE('',#5139,#5136,#2919,.T.);
#6306=EDGE_CURVE('',#5140,#4965,#2920,.T.);
#6307=EDGE_CURVE('',#5141,#5140,#2921,.T.);
#6308=EDGE_CURVE('',#5141,#4964,#2922,.T.);
#6309=EDGE_CURVE('',#4966,#5142,#2923,.T.);
#6310=EDGE_CURVE('',#5142,#5143,#2924,.T.);
#6311=EDGE_CURVE('',#4967,#5143,#2925,.T.);
#6312=EDGE_CURVE('',#5142,#5141,#2926,.T.);
#6313=EDGE_CURVE('',#5143,#5140,#2927,.T.);
#6314=EDGE_CURVE('',#5144,#4969,#2928,.T.);
#6315=EDGE_CURVE('',#5145,#5144,#2929,.T.);
#6316=EDGE_CURVE('',#5145,#4968,#2930,.T.);
#6317=EDGE_CURVE('',#4970,#5146,#2931,.T.);
#6318=EDGE_CURVE('',#5146,#5147,#2932,.T.);
#6319=EDGE_CURVE('',#4971,#5147,#2933,.T.);
#6320=EDGE_CURVE('',#5146,#5145,#2934,.T.);
#6321=EDGE_CURVE('',#5147,#5144,#2935,.T.);
#6322=EDGE_CURVE('',#5148,#4989,#2936,.T.);
#6323=EDGE_CURVE('',#5149,#5148,#2937,.T.);
#6324=EDGE_CURVE('',#5149,#4988,#2938,.T.);
#6325=EDGE_CURVE('',#4990,#5150,#2939,.T.);
#6326=EDGE_CURVE('',#5150,#5151,#2940,.T.);
#6327=EDGE_CURVE('',#4991,#5151,#2941,.T.);
#6328=EDGE_CURVE('',#5150,#5149,#2942,.T.);
#6329=EDGE_CURVE('',#5151,#5148,#2943,.T.);
#6330=EDGE_CURVE('',#5152,#4993,#2944,.T.);
#6331=EDGE_CURVE('',#5153,#5152,#2945,.T.);
#6332=EDGE_CURVE('',#5153,#4992,#2946,.T.);
#6333=EDGE_CURVE('',#4994,#5154,#2947,.T.);
#6334=EDGE_CURVE('',#5154,#5155,#2948,.T.);
#6335=EDGE_CURVE('',#4995,#5155,#2949,.T.);
#6336=EDGE_CURVE('',#5154,#5153,#2950,.T.);
#6337=EDGE_CURVE('',#5155,#5152,#2951,.T.);
#6338=EDGE_CURVE('',#5156,#4997,#2952,.T.);
#6339=EDGE_CURVE('',#5157,#5156,#2953,.T.);
#6340=EDGE_CURVE('',#5157,#4996,#2954,.T.);
#6341=EDGE_CURVE('',#4998,#5158,#2955,.T.);
#6342=EDGE_CURVE('',#5158,#5159,#2956,.T.);
#6343=EDGE_CURVE('',#4999,#5159,#2957,.T.);
#6344=EDGE_CURVE('',#5158,#5157,#2958,.T.);
#6345=EDGE_CURVE('',#5159,#5156,#2959,.T.);
#6346=EDGE_CURVE('',#5160,#5001,#2960,.T.);
#6347=EDGE_CURVE('',#5161,#5160,#2961,.T.);
#6348=EDGE_CURVE('',#5161,#5000,#2962,.T.);
#6349=EDGE_CURVE('',#5002,#5162,#2963,.T.);
#6350=EDGE_CURVE('',#5162,#5163,#2964,.T.);
#6351=EDGE_CURVE('',#5003,#5163,#2965,.T.);
#6352=EDGE_CURVE('',#5162,#5161,#2966,.T.);
#6353=EDGE_CURVE('',#5163,#5160,#2967,.T.);
#6354=EDGE_CURVE('',#5164,#5005,#2968,.T.);
#6355=EDGE_CURVE('',#5165,#5164,#2969,.T.);
#6356=EDGE_CURVE('',#5165,#5004,#2970,.T.);
#6357=EDGE_CURVE('',#5006,#5166,#2971,.T.);
#6358=EDGE_CURVE('',#5166,#5167,#2972,.T.);
#6359=EDGE_CURVE('',#5007,#5167,#2973,.T.);
#6360=EDGE_CURVE('',#5166,#5165,#2974,.T.);
#6361=EDGE_CURVE('',#5167,#5164,#2975,.T.);
#6362=EDGE_CURVE('',#5168,#5009,#2976,.T.);
#6363=EDGE_CURVE('',#5169,#5168,#2977,.T.);
#6364=EDGE_CURVE('',#5169,#5008,#2978,.T.);
#6365=EDGE_CURVE('',#5010,#5170,#2979,.T.);
#6366=EDGE_CURVE('',#5170,#5171,#2980,.T.);
#6367=EDGE_CURVE('',#5011,#5171,#2981,.T.);
#6368=EDGE_CURVE('',#5170,#5169,#2982,.T.);
#6369=EDGE_CURVE('',#5171,#5168,#2983,.T.);
#6370=EDGE_CURVE('',#5172,#5013,#2984,.T.);
#6371=EDGE_CURVE('',#5173,#5172,#2985,.T.);
#6372=EDGE_CURVE('',#5173,#5012,#2986,.T.);
#6373=EDGE_CURVE('',#5014,#5174,#2987,.T.);
#6374=EDGE_CURVE('',#5174,#5175,#2988,.T.);
#6375=EDGE_CURVE('',#5015,#5175,#2989,.T.);
#6376=EDGE_CURVE('',#5174,#5173,#2990,.T.);
#6377=EDGE_CURVE('',#5175,#5172,#2991,.T.);
#6378=EDGE_CURVE('',#5176,#5017,#2992,.T.);
#6379=EDGE_CURVE('',#5177,#5176,#2993,.T.);
#6380=EDGE_CURVE('',#5177,#5016,#2994,.T.);
#6381=EDGE_CURVE('',#5018,#5178,#2995,.T.);
#6382=EDGE_CURVE('',#5178,#5179,#2996,.T.);
#6383=EDGE_CURVE('',#5019,#5179,#2997,.T.);
#6384=EDGE_CURVE('',#5178,#5177,#2998,.T.);
#6385=EDGE_CURVE('',#5179,#5176,#2999,.T.);
#6386=EDGE_CURVE('',#5180,#5021,#3000,.T.);
#6387=EDGE_CURVE('',#5181,#5180,#3001,.T.);
#6388=EDGE_CURVE('',#5181,#5020,#3002,.T.);
#6389=EDGE_CURVE('',#5022,#5182,#3003,.T.);
#6390=EDGE_CURVE('',#5182,#5183,#3004,.T.);
#6391=EDGE_CURVE('',#5023,#5183,#3005,.T.);
#6392=EDGE_CURVE('',#5182,#5181,#3006,.T.);
#6393=EDGE_CURVE('',#5183,#5180,#3007,.T.);
#6394=EDGE_CURVE('',#5184,#5025,#3008,.T.);
#6395=EDGE_CURVE('',#5185,#5184,#3009,.T.);
#6396=EDGE_CURVE('',#5185,#5024,#3010,.T.);
#6397=EDGE_CURVE('',#5026,#5186,#3011,.T.);
#6398=EDGE_CURVE('',#5186,#5187,#3012,.T.);
#6399=EDGE_CURVE('',#5027,#5187,#3013,.T.);
#6400=EDGE_CURVE('',#5186,#5185,#3014,.T.);
#6401=EDGE_CURVE('',#5187,#5184,#3015,.T.);
#6402=EDGE_CURVE('',#5188,#5029,#3016,.T.);
#6403=EDGE_CURVE('',#5189,#5188,#3017,.T.);
#6404=EDGE_CURVE('',#5189,#5028,#3018,.T.);
#6405=EDGE_CURVE('',#5030,#5190,#3019,.T.);
#6406=EDGE_CURVE('',#5190,#5191,#3020,.T.);
#6407=EDGE_CURVE('',#5031,#5191,#3021,.T.);
#6408=EDGE_CURVE('',#5190,#5189,#3022,.T.);
#6409=EDGE_CURVE('',#5191,#5188,#3023,.T.);
#6410=EDGE_CURVE('',#5192,#5033,#3024,.T.);
#6411=EDGE_CURVE('',#5193,#5192,#3025,.T.);
#6412=EDGE_CURVE('',#5193,#5032,#3026,.T.);
#6413=EDGE_CURVE('',#5034,#5194,#3027,.T.);
#6414=EDGE_CURVE('',#5194,#5195,#3028,.T.);
#6415=EDGE_CURVE('',#5035,#5195,#3029,.T.);
#6416=EDGE_CURVE('',#5194,#5193,#3030,.T.);
#6417=EDGE_CURVE('',#5195,#5192,#3031,.T.);
#6418=EDGE_CURVE('',#5196,#5037,#3032,.T.);
#6419=EDGE_CURVE('',#5197,#5196,#3033,.T.);
#6420=EDGE_CURVE('',#5197,#5036,#3034,.T.);
#6421=EDGE_CURVE('',#5038,#5198,#3035,.T.);
#6422=EDGE_CURVE('',#5198,#5199,#3036,.T.);
#6423=EDGE_CURVE('',#5039,#5199,#3037,.T.);
#6424=EDGE_CURVE('',#5198,#5197,#3038,.T.);
#6425=EDGE_CURVE('',#5199,#5196,#3039,.T.);
#6426=EDGE_CURVE('',#5200,#5041,#3040,.T.);
#6427=EDGE_CURVE('',#5201,#5200,#3041,.T.);
#6428=EDGE_CURVE('',#5201,#5040,#3042,.T.);
#6429=EDGE_CURVE('',#5042,#5202,#3043,.T.);
#6430=EDGE_CURVE('',#5202,#5203,#3044,.T.);
#6431=EDGE_CURVE('',#5043,#5203,#3045,.T.);
#6432=EDGE_CURVE('',#5202,#5201,#3046,.T.);
#6433=EDGE_CURVE('',#5203,#5200,#3047,.T.);
#6434=EDGE_CURVE('',#5204,#5045,#3048,.T.);
#6435=EDGE_CURVE('',#5205,#5204,#3049,.T.);
#6436=EDGE_CURVE('',#5205,#5044,#3050,.T.);
#6437=EDGE_CURVE('',#5046,#5206,#3051,.T.);
#6438=EDGE_CURVE('',#5206,#5207,#3052,.T.);
#6439=EDGE_CURVE('',#5047,#5207,#3053,.T.);
#6440=EDGE_CURVE('',#5206,#5205,#3054,.T.);
#6441=EDGE_CURVE('',#5207,#5204,#3055,.T.);
#6442=EDGE_CURVE('',#5208,#5208,#4428,.T.);
#6443=EDGE_CURVE('',#5208,#5209,#3056,.T.);
#6444=EDGE_CURVE('',#5209,#5209,#4429,.T.);
#6445=EDGE_CURVE('',#5210,#5210,#4430,.T.);
#6446=EDGE_CURVE('',#5210,#5211,#3057,.T.);
#6447=EDGE_CURVE('',#5211,#5211,#4431,.T.);
#6448=EDGE_CURVE('',#5212,#5213,#3058,.T.);
#6449=EDGE_CURVE('',#5213,#5214,#3059,.T.);
#6450=EDGE_CURVE('',#5214,#5215,#3060,.T.);
#6451=EDGE_CURVE('',#5215,#5216,#3061,.T.);
#6452=EDGE_CURVE('',#5216,#5217,#3062,.T.);
#6453=EDGE_CURVE('',#5217,#5218,#3063,.T.);
#6454=EDGE_CURVE('',#5218,#5219,#3064,.T.);
#6455=EDGE_CURVE('',#5219,#5220,#3065,.T.);
#6456=EDGE_CURVE('',#5220,#5221,#3066,.T.);
#6457=EDGE_CURVE('',#5221,#5222,#3067,.T.);
#6458=EDGE_CURVE('',#5222,#5223,#3068,.T.);
#6459=EDGE_CURVE('',#5223,#5224,#3069,.T.);
#6460=EDGE_CURVE('',#5224,#5225,#3070,.T.);
#6461=EDGE_CURVE('',#5225,#5212,#3071,.T.);
#6462=EDGE_CURVE('',#5226,#5227,#3072,.T.);
#6463=EDGE_CURVE('',#5228,#5226,#3073,.T.);
#6464=EDGE_CURVE('',#5229,#5228,#3074,.T.);
#6465=EDGE_CURVE('',#5230,#5229,#3075,.T.);
#6466=EDGE_CURVE('',#5231,#5230,#3076,.T.);
#6467=EDGE_CURVE('',#5232,#5231,#3077,.T.);
#6468=EDGE_CURVE('',#5233,#5232,#3078,.T.);
#6469=EDGE_CURVE('',#5234,#5233,#3079,.T.);
#6470=EDGE_CURVE('',#5235,#5234,#3080,.T.);
#6471=EDGE_CURVE('',#5236,#5235,#3081,.T.);
#6472=EDGE_CURVE('',#5237,#5236,#3082,.T.);
#6473=EDGE_CURVE('',#5238,#5237,#3083,.T.);
#6474=EDGE_CURVE('',#5239,#5238,#3084,.T.);
#6475=EDGE_CURVE('',#5227,#5239,#3085,.T.);
#6476=EDGE_CURVE('',#5213,#5227,#3086,.T.);
#6477=EDGE_CURVE('',#5212,#5226,#3087,.T.);
#6478=EDGE_CURVE('',#5214,#5239,#3088,.T.);
#6479=EDGE_CURVE('',#5215,#5238,#3089,.T.);
#6480=EDGE_CURVE('',#5216,#5237,#3090,.T.);
#6481=EDGE_CURVE('',#5217,#5236,#3091,.T.);
#6482=EDGE_CURVE('',#5218,#5235,#3092,.T.);
#6483=EDGE_CURVE('',#5219,#5234,#3093,.T.);
#6484=EDGE_CURVE('',#5220,#5233,#3094,.T.);
#6485=EDGE_CURVE('',#5221,#5232,#3095,.T.);
#6486=EDGE_CURVE('',#5222,#5231,#3096,.T.);
#6487=EDGE_CURVE('',#5223,#5230,#3097,.T.);
#6488=EDGE_CURVE('',#5224,#5229,#3098,.T.);
#6489=EDGE_CURVE('',#5225,#5228,#3099,.T.);
#6490=EDGE_CURVE('',#5240,#5240,#4432,.T.);
#6491=EDGE_CURVE('',#5240,#5241,#3100,.T.);
#6492=EDGE_CURVE('',#5241,#5241,#4433,.T.);
#6493=EDGE_CURVE('',#5242,#5243,#4434,.T.);
#6494=EDGE_CURVE('',#5243,#5242,#4435,.T.);
#6495=EDGE_CURVE('',#5243,#5240,#3101,.T.);
#6496=EDGE_CURVE('',#5242,#5244,#3102,.T.);
#6497=EDGE_CURVE('',#5244,#5244,#4436,.T.);
#6498=EDGE_CURVE('',#5245,#5245,#4437,.T.);
#6499=EDGE_CURVE('',#5245,#5246,#3103,.T.);
#6500=EDGE_CURVE('',#5246,#5246,#4438,.T.);
#6501=EDGE_CURVE('',#5247,#5247,#4439,.T.);
#6502=EDGE_CURVE('',#5247,#5248,#3104,.T.);
#6503=EDGE_CURVE('',#5248,#5248,#4440,.T.);
#6504=EDGE_CURVE('',#5249,#5249,#4441,.T.);
#6505=EDGE_CURVE('',#5249,#5250,#3105,.T.);
#6506=EDGE_CURVE('',#5250,#5250,#4442,.T.);
#6507=EDGE_CURVE('',#5251,#5251,#4443,.T.);
#6508=EDGE_CURVE('',#5251,#5252,#3106,.T.);
#6509=EDGE_CURVE('',#5252,#5252,#4444,.T.);
#6510=EDGE_CURVE('',#5253,#5254,#3107,.T.);
#6511=EDGE_CURVE('',#5254,#5255,#3108,.T.);
#6512=EDGE_CURVE('',#5255,#5256,#3109,.T.);
#6513=EDGE_CURVE('',#5256,#5257,#3110,.T.);
#6514=EDGE_CURVE('',#5257,#5258,#3111,.T.);
#6515=EDGE_CURVE('',#5258,#5253,#3112,.T.);
#6516=EDGE_CURVE('',#5259,#5260,#3113,.T.);
#6517=EDGE_CURVE('',#5261,#5259,#3114,.T.);
#6518=EDGE_CURVE('',#5262,#5261,#3115,.T.);
#6519=EDGE_CURVE('',#5263,#5262,#3116,.T.);
#6520=EDGE_CURVE('',#5264,#5263,#3117,.T.);
#6521=EDGE_CURVE('',#5260,#5264,#3118,.T.);
#6522=EDGE_CURVE('',#5254,#5260,#3119,.T.);
#6523=EDGE_CURVE('',#5253,#5259,#3120,.T.);
#6524=EDGE_CURVE('',#5255,#5264,#3121,.T.);
#6525=EDGE_CURVE('',#5256,#5263,#3122,.T.);
#6526=EDGE_CURVE('',#5257,#5262,#3123,.T.);
#6527=EDGE_CURVE('',#5258,#5261,#3124,.T.);
#6528=EDGE_CURVE('',#5265,#5265,#4445,.T.);
#6529=EDGE_CURVE('',#5265,#5266,#3125,.T.);
#6530=EDGE_CURVE('',#5266,#5266,#4446,.T.);
#6531=EDGE_CURVE('',#5267,#5267,#4447,.T.);
#6532=EDGE_CURVE('',#5267,#5268,#3126,.T.);
#6533=EDGE_CURVE('',#5268,#5268,#4448,.T.);
#6534=EDGE_CURVE('',#5269,#5270,#3127,.T.);
#6535=EDGE_CURVE('',#5271,#5269,#3128,.T.);
#6536=EDGE_CURVE('',#5272,#5271,#3129,.T.);
#6537=EDGE_CURVE('',#5273,#5272,#3130,.T.);
#6538=EDGE_CURVE('',#5274,#5273,#3131,.T.);
#6539=EDGE_CURVE('',#5270,#5274,#3132,.T.);
#6540=EDGE_CURVE('',#5275,#5270,#3133,.T.);
#6541=EDGE_CURVE('',#5275,#5276,#3134,.T.);
#6542=EDGE_CURVE('',#5276,#5269,#3135,.T.);
#6543=EDGE_CURVE('',#5276,#5277,#3136,.T.);
#6544=EDGE_CURVE('',#5277,#5271,#3137,.T.);
#6545=EDGE_CURVE('',#5277,#5278,#3138,.T.);
#6546=EDGE_CURVE('',#5278,#5272,#3139,.T.);
#6547=EDGE_CURVE('',#5278,#5279,#3140,.T.);
#6548=EDGE_CURVE('',#5279,#5273,#3141,.T.);
#6549=EDGE_CURVE('',#5279,#5280,#3142,.T.);
#6550=EDGE_CURVE('',#5280,#5274,#3143,.T.);
#6551=EDGE_CURVE('',#5280,#5275,#3144,.T.);
#6552=EDGE_CURVE('',#5281,#5281,#4449,.T.);
#6553=EDGE_CURVE('',#5281,#5282,#3145,.T.);
#6554=EDGE_CURVE('',#5282,#5282,#4450,.T.);
#6555=EDGE_CURVE('',#5283,#5284,#3146,.T.);
#6556=EDGE_CURVE('',#5285,#5284,#3147,.T.);
#6557=EDGE_CURVE('',#5286,#5285,#3148,.T.);
#6558=EDGE_CURVE('',#5286,#5283,#3149,.T.);
#6559=EDGE_CURVE('',#5284,#5287,#3150,.T.);
#6560=EDGE_CURVE('',#5288,#5287,#3151,.T.);
#6561=EDGE_CURVE('',#5285,#5288,#3152,.T.);
#6562=EDGE_CURVE('',#5287,#5289,#3153,.T.);
#6563=EDGE_CURVE('',#5290,#5289,#3154,.T.);
#6564=EDGE_CURVE('',#5288,#5290,#3155,.T.);
#6565=EDGE_CURVE('',#5289,#5291,#3156,.T.);
#6566=EDGE_CURVE('',#5292,#5291,#3157,.T.);
#6567=EDGE_CURVE('',#5290,#5292,#3158,.T.);
#6568=EDGE_CURVE('',#5291,#5293,#3159,.T.);
#6569=EDGE_CURVE('',#5294,#5293,#3160,.T.);
#6570=EDGE_CURVE('',#5292,#5294,#3161,.T.);
#6571=EDGE_CURVE('',#5293,#5283,#3162,.T.);
#6572=EDGE_CURVE('',#5294,#5286,#3163,.T.);
#6573=EDGE_CURVE('',#5295,#5295,#4451,.T.);
#6574=EDGE_CURVE('',#5295,#5296,#3164,.T.);
#6575=EDGE_CURVE('',#5296,#5296,#4452,.T.);
#6576=EDGE_CURVE('',#5297,#5297,#4453,.T.);
#6577=EDGE_CURVE('',#5297,#5298,#3165,.T.);
#6578=EDGE_CURVE('',#5298,#5298,#4454,.T.);
#6579=EDGE_CURVE('',#5299,#5300,#3166,.T.);
#6580=EDGE_CURVE('',#5301,#5299,#3167,.T.);
#6581=EDGE_CURVE('',#5302,#5301,#3168,.T.);
#6582=EDGE_CURVE('',#5303,#5302,#3169,.T.);
#6583=EDGE_CURVE('',#5304,#5303,#3170,.T.);
#6584=EDGE_CURVE('',#5300,#5304,#3171,.T.);
#6585=EDGE_CURVE('',#5305,#5300,#3172,.T.);
#6586=EDGE_CURVE('',#5305,#5306,#3173,.T.);
#6587=EDGE_CURVE('',#5306,#5299,#3174,.T.);
#6588=EDGE_CURVE('',#5306,#5307,#3175,.T.);
#6589=EDGE_CURVE('',#5307,#5301,#3176,.T.);
#6590=EDGE_CURVE('',#5307,#5308,#3177,.T.);
#6591=EDGE_CURVE('',#5308,#5302,#3178,.T.);
#6592=EDGE_CURVE('',#5308,#5309,#3179,.T.);
#6593=EDGE_CURVE('',#5309,#5303,#3180,.T.);
#6594=EDGE_CURVE('',#5309,#5310,#3181,.T.);
#6595=EDGE_CURVE('',#5310,#5304,#3182,.T.);
#6596=EDGE_CURVE('',#5310,#5305,#3183,.T.);
#6597=ORIENTED_EDGE('',*,*,#5311,.T.);
#6598=ORIENTED_EDGE('',*,*,#5312,.T.);
#6599=ORIENTED_EDGE('',*,*,#5313,.T.);
#6600=ORIENTED_EDGE('',*,*,#5312,.F.);
#6601=ORIENTED_EDGE('',*,*,#5314,.T.);
#6602=ORIENTED_EDGE('',*,*,#5315,.T.);
#6603=ORIENTED_EDGE('',*,*,#5316,.F.);
#6604=ORIENTED_EDGE('',*,*,#5315,.F.);
#6605=ORIENTED_EDGE('',*,*,#5317,.F.);
#6606=ORIENTED_EDGE('',*,*,#5318,.T.);
#6607=ORIENTED_EDGE('',*,*,#5319,.T.);
#6608=ORIENTED_EDGE('',*,*,#5320,.F.);
#6609=ORIENTED_EDGE('',*,*,#5321,.F.);
#6610=ORIENTED_EDGE('',*,*,#5322,.F.);
#6611=ORIENTED_EDGE('',*,*,#5323,.T.);
#6612=ORIENTED_EDGE('',*,*,#5324,.F.);
#6613=ORIENTED_EDGE('',*,*,#5325,.F.);
#6614=ORIENTED_EDGE('',*,*,#5326,.F.);
#6615=ORIENTED_EDGE('',*,*,#5327,.T.);
#6616=ORIENTED_EDGE('',*,*,#5328,.F.);
#6617=ORIENTED_EDGE('',*,*,#5329,.F.);
#6618=ORIENTED_EDGE('',*,*,#5330,.F.);
#6619=ORIENTED_EDGE('',*,*,#5331,.T.);
#6620=ORIENTED_EDGE('',*,*,#5332,.T.);
#6621=ORIENTED_EDGE('',*,*,#5333,.T.);
#6622=ORIENTED_EDGE('',*,*,#5334,.F.);
#6623=ORIENTED_EDGE('',*,*,#5335,.F.);
#6624=ORIENTED_EDGE('',*,*,#5336,.F.);
#6625=ORIENTED_EDGE('',*,*,#5337,.T.);
#6626=ORIENTED_EDGE('',*,*,#5338,.F.);
#6627=ORIENTED_EDGE('',*,*,#5339,.F.);
#6628=ORIENTED_EDGE('',*,*,#5340,.F.);
#6629=ORIENTED_EDGE('',*,*,#5341,.T.);
#6630=ORIENTED_EDGE('',*,*,#5342,.F.);
#6631=ORIENTED_EDGE('',*,*,#5343,.F.);
#6632=ORIENTED_EDGE('',*,*,#5344,.F.);
#6633=ORIENTED_EDGE('',*,*,#5345,.T.);
#6634=ORIENTED_EDGE('',*,*,#5346,.T.);
#6635=ORIENTED_EDGE('',*,*,#5347,.F.);
#6636=ORIENTED_EDGE('',*,*,#5348,.T.);
#6637=ORIENTED_EDGE('',*,*,#5349,.F.);
#6638=ORIENTED_EDGE('',*,*,#5350,.T.);
#6639=ORIENTED_EDGE('',*,*,#5351,.T.);
#6640=ORIENTED_EDGE('',*,*,#5352,.F.);
#6641=ORIENTED_EDGE('',*,*,#5353,.F.);
#6642=ORIENTED_EDGE('',*,*,#5354,.F.);
#6643=ORIENTED_EDGE('',*,*,#5355,.T.);
#6644=ORIENTED_EDGE('',*,*,#5356,.T.);
#6645=ORIENTED_EDGE('',*,*,#5357,.F.);
#6646=ORIENTED_EDGE('',*,*,#5337,.F.);
#6647=ORIENTED_EDGE('',*,*,#5358,.F.);
#6648=ORIENTED_EDGE('',*,*,#5359,.T.);
#6649=ORIENTED_EDGE('',*,*,#5360,.F.);
#6650=ORIENTED_EDGE('',*,*,#5361,.T.);
#6651=ORIENTED_EDGE('',*,*,#5362,.F.);
#6652=ORIENTED_EDGE('',*,*,#5341,.F.);
#6653=ORIENTED_EDGE('',*,*,#5363,.F.);
#6654=ORIENTED_EDGE('',*,*,#5364,.T.);
#6655=ORIENTED_EDGE('',*,*,#5365,.F.);
#6656=ORIENTED_EDGE('',*,*,#5345,.F.);
#6657=ORIENTED_EDGE('',*,*,#5366,.F.);
#6658=ORIENTED_EDGE('',*,*,#5333,.F.);
#6659=ORIENTED_EDGE('',*,*,#5367,.T.);
#6660=ORIENTED_EDGE('',*,*,#5368,.T.);
#6661=ORIENTED_EDGE('',*,*,#5369,.F.);
#6662=ORIENTED_EDGE('',*,*,#5370,.T.);
#6663=ORIENTED_EDGE('',*,*,#5371,.F.);
#6664=ORIENTED_EDGE('',*,*,#5331,.F.);
#6665=ORIENTED_EDGE('',*,*,#5372,.F.);
#6666=ORIENTED_EDGE('',*,*,#5327,.F.);
#6667=ORIENTED_EDGE('',*,*,#5373,.F.);
#6668=ORIENTED_EDGE('',*,*,#5374,.T.);
#6669=ORIENTED_EDGE('',*,*,#5375,.F.);
#6670=ORIENTED_EDGE('',*,*,#5323,.F.);
#6671=ORIENTED_EDGE('',*,*,#5376,.F.);
#6672=ORIENTED_EDGE('',*,*,#5377,.T.);
#6673=ORIENTED_EDGE('',*,*,#5378,.F.);
#6674=ORIENTED_EDGE('',*,*,#5319,.F.);
#6675=ORIENTED_EDGE('',*,*,#5379,.T.);
#6676=ORIENTED_EDGE('',*,*,#5380,.T.);
#6677=ORIENTED_EDGE('',*,*,#5370,.F.);
#6678=ORIENTED_EDGE('',*,*,#5381,.T.);
#6679=ORIENTED_EDGE('',*,*,#5382,.T.);
#6680=ORIENTED_EDGE('',*,*,#5383,.T.);
#6681=ORIENTED_EDGE('',*,*,#5374,.F.);
#6682=ORIENTED_EDGE('',*,*,#5384,.T.);
#6683=ORIENTED_EDGE('',*,*,#5385,.T.);
#6684=ORIENTED_EDGE('',*,*,#5386,.T.);
#6685=ORIENTED_EDGE('',*,*,#5377,.F.);
#6686=ORIENTED_EDGE('',*,*,#5387,.T.);
#6687=ORIENTED_EDGE('',*,*,#5388,.T.);
#6688=ORIENTED_EDGE('',*,*,#5389,.T.);
#6689=ORIENTED_EDGE('',*,*,#5380,.F.);
#6690=ORIENTED_EDGE('',*,*,#5390,.F.);
#6691=ORIENTED_EDGE('',*,*,#5364,.F.);
#6692=ORIENTED_EDGE('',*,*,#5391,.T.);
#6693=ORIENTED_EDGE('',*,*,#5392,.T.);
#6694=ORIENTED_EDGE('',*,*,#5393,.T.);
#6695=ORIENTED_EDGE('',*,*,#5361,.F.);
#6696=ORIENTED_EDGE('',*,*,#5394,.T.);
#6697=ORIENTED_EDGE('',*,*,#5395,.T.);
#6698=ORIENTED_EDGE('',*,*,#5396,.T.);
#6699=ORIENTED_EDGE('',*,*,#5359,.F.);
#6700=ORIENTED_EDGE('',*,*,#5397,.T.);
#6701=ORIENTED_EDGE('',*,*,#5398,.T.);
#6702=ORIENTED_EDGE('',*,*,#5399,.T.);
#6703=ORIENTED_EDGE('',*,*,#5368,.F.);
#6704=ORIENTED_EDGE('',*,*,#5400,.F.);
#6705=ORIENTED_EDGE('',*,*,#5400,.T.);
#6706=ORIENTED_EDGE('',*,*,#5367,.F.);
#6707=ORIENTED_EDGE('',*,*,#5332,.F.);
#6708=ORIENTED_EDGE('',*,*,#5371,.T.);
#6709=ORIENTED_EDGE('',*,*,#5401,.F.);
#6710=ORIENTED_EDGE('',*,*,#5346,.F.);
#6711=ORIENTED_EDGE('',*,*,#5365,.T.);
#6712=ORIENTED_EDGE('',*,*,#5390,.T.);
#6713=ORIENTED_EDGE('',*,*,#5379,.F.);
#6714=ORIENTED_EDGE('',*,*,#5318,.F.);
#6715=ORIENTED_EDGE('',*,*,#5402,.T.);
#6716=ORIENTED_EDGE('',*,*,#5355,.F.);
#6717=ORIENTED_EDGE('',*,*,#5403,.F.);
#6718=ORIENTED_EDGE('',*,*,#5404,.T.);
#6719=ORIENTED_EDGE('',*,*,#5405,.T.);
#6720=ORIENTED_EDGE('',*,*,#5406,.F.);
#6721=ORIENTED_EDGE('',*,*,#5407,.F.);
#6722=ORIENTED_EDGE('',*,*,#5353,.T.);
#6723=ORIENTED_EDGE('',*,*,#5408,.T.);
#6724=ORIENTED_EDGE('',*,*,#5409,.F.);
#6725=ORIENTED_EDGE('',*,*,#5410,.F.);
#6726=ORIENTED_EDGE('',*,*,#5406,.T.);
#6727=ORIENTED_EDGE('',*,*,#5411,.T.);
#6728=ORIENTED_EDGE('',*,*,#5404,.F.);
#6729=ORIENTED_EDGE('',*,*,#5412,.F.);
#6730=ORIENTED_EDGE('',*,*,#5409,.T.);
#6731=ORIENTED_EDGE('',*,*,#5403,.T.);
#6732=ORIENTED_EDGE('',*,*,#5354,.T.);
#6733=ORIENTED_EDGE('',*,*,#5407,.T.);
#6734=ORIENTED_EDGE('',*,*,#5410,.T.);
#6735=ORIENTED_EDGE('',*,*,#5412,.T.);
#6736=ORIENTED_EDGE('',*,*,#5402,.F.);
#6737=ORIENTED_EDGE('',*,*,#5411,.F.);
#6738=ORIENTED_EDGE('',*,*,#5408,.F.);
#6739=ORIENTED_EDGE('',*,*,#5405,.F.);
#6740=ORIENTED_EDGE('',*,*,#5356,.F.);
#6741=ORIENTED_EDGE('',*,*,#5313,.F.);
#6742=ORIENTED_EDGE('',*,*,#5413,.T.);
#6743=ORIENTED_EDGE('',*,*,#5414,.F.);
#6744=ORIENTED_EDGE('',*,*,#5415,.F.);
#6745=ORIENTED_EDGE('',*,*,#5352,.T.);
#6746=ORIENTED_EDGE('',*,*,#5416,.T.);
#6747=ORIENTED_EDGE('',*,*,#5417,.F.);
#6748=ORIENTED_EDGE('',*,*,#5418,.F.);
#6749=ORIENTED_EDGE('',*,*,#5414,.T.);
#6750=ORIENTED_EDGE('',*,*,#5419,.T.);
#6751=ORIENTED_EDGE('',*,*,#5420,.F.);
#6752=ORIENTED_EDGE('',*,*,#5421,.F.);
#6753=ORIENTED_EDGE('',*,*,#5417,.T.);
#6754=ORIENTED_EDGE('',*,*,#5422,.T.);
#6755=ORIENTED_EDGE('',*,*,#5350,.F.);
#6756=ORIENTED_EDGE('',*,*,#5423,.F.);
#6757=ORIENTED_EDGE('',*,*,#5420,.T.);
#6758=ORIENTED_EDGE('',*,*,#5415,.T.);
#6759=ORIENTED_EDGE('',*,*,#5418,.T.);
#6760=ORIENTED_EDGE('',*,*,#5421,.T.);
#6761=ORIENTED_EDGE('',*,*,#5423,.T.);
#6762=ORIENTED_EDGE('',*,*,#5349,.T.);
#6763=ORIENTED_EDGE('',*,*,#5413,.F.);
#6764=ORIENTED_EDGE('',*,*,#5351,.F.);
#6765=ORIENTED_EDGE('',*,*,#5422,.F.);
#6766=ORIENTED_EDGE('',*,*,#5419,.F.);
#6767=ORIENTED_EDGE('',*,*,#5416,.F.);
#6768=ORIENTED_EDGE('',*,*,#5316,.T.);
#6769=ORIENTED_EDGE('',*,*,#5322,.T.);
#6770=ORIENTED_EDGE('',*,*,#5424,.T.);
#6771=ORIENTED_EDGE('',*,*,#5387,.F.);
#6772=ORIENTED_EDGE('',*,*,#5376,.T.);
#6773=ORIENTED_EDGE('',*,*,#5321,.T.);
#6774=ORIENTED_EDGE('',*,*,#5425,.T.);
#6775=ORIENTED_EDGE('',*,*,#5388,.F.);
#6776=ORIENTED_EDGE('',*,*,#5424,.F.);
#6777=ORIENTED_EDGE('',*,*,#5320,.T.);
#6778=ORIENTED_EDGE('',*,*,#5378,.T.);
#6779=ORIENTED_EDGE('',*,*,#5389,.F.);
#6780=ORIENTED_EDGE('',*,*,#5425,.F.);
#6781=ORIENTED_EDGE('',*,*,#5334,.T.);
#6782=ORIENTED_EDGE('',*,*,#5366,.T.);
#6783=ORIENTED_EDGE('',*,*,#5399,.F.);
#6784=ORIENTED_EDGE('',*,*,#5426,.F.);
#6785=ORIENTED_EDGE('',*,*,#5336,.T.);
#6786=ORIENTED_EDGE('',*,*,#5427,.T.);
#6787=ORIENTED_EDGE('',*,*,#5397,.F.);
#6788=ORIENTED_EDGE('',*,*,#5358,.T.);
#6789=ORIENTED_EDGE('',*,*,#5335,.T.);
#6790=ORIENTED_EDGE('',*,*,#5426,.T.);
#6791=ORIENTED_EDGE('',*,*,#5398,.F.);
#6792=ORIENTED_EDGE('',*,*,#5427,.F.);
#6793=ORIENTED_EDGE('',*,*,#5342,.T.);
#6794=ORIENTED_EDGE('',*,*,#5362,.T.);
#6795=ORIENTED_EDGE('',*,*,#5393,.F.);
#6796=ORIENTED_EDGE('',*,*,#5428,.F.);
#6797=ORIENTED_EDGE('',*,*,#5344,.T.);
#6798=ORIENTED_EDGE('',*,*,#5429,.T.);
#6799=ORIENTED_EDGE('',*,*,#5391,.F.);
#6800=ORIENTED_EDGE('',*,*,#5363,.T.);
#6801=ORIENTED_EDGE('',*,*,#5343,.T.);
#6802=ORIENTED_EDGE('',*,*,#5428,.T.);
#6803=ORIENTED_EDGE('',*,*,#5392,.F.);
#6804=ORIENTED_EDGE('',*,*,#5429,.F.);
#6805=ORIENTED_EDGE('',*,*,#5326,.T.);
#6806=ORIENTED_EDGE('',*,*,#5430,.T.);
#6807=ORIENTED_EDGE('',*,*,#5384,.F.);
#6808=ORIENTED_EDGE('',*,*,#5373,.T.);
#6809=ORIENTED_EDGE('',*,*,#5325,.T.);
#6810=ORIENTED_EDGE('',*,*,#5431,.T.);
#6811=ORIENTED_EDGE('',*,*,#5385,.F.);
#6812=ORIENTED_EDGE('',*,*,#5430,.F.);
#6813=ORIENTED_EDGE('',*,*,#5324,.T.);
#6814=ORIENTED_EDGE('',*,*,#5375,.T.);
#6815=ORIENTED_EDGE('',*,*,#5386,.F.);
#6816=ORIENTED_EDGE('',*,*,#5431,.F.);
#6817=ORIENTED_EDGE('',*,*,#5338,.T.);
#6818=ORIENTED_EDGE('',*,*,#5357,.T.);
#6819=ORIENTED_EDGE('',*,*,#5396,.F.);
#6820=ORIENTED_EDGE('',*,*,#5432,.F.);
#6821=ORIENTED_EDGE('',*,*,#5340,.T.);
#6822=ORIENTED_EDGE('',*,*,#5433,.T.);
#6823=ORIENTED_EDGE('',*,*,#5394,.F.);
#6824=ORIENTED_EDGE('',*,*,#5360,.T.);
#6825=ORIENTED_EDGE('',*,*,#5339,.T.);
#6826=ORIENTED_EDGE('',*,*,#5432,.T.);
#6827=ORIENTED_EDGE('',*,*,#5395,.F.);
#6828=ORIENTED_EDGE('',*,*,#5433,.F.);
#6829=ORIENTED_EDGE('',*,*,#5330,.T.);
#6830=ORIENTED_EDGE('',*,*,#5434,.T.);
#6831=ORIENTED_EDGE('',*,*,#5381,.F.);
#6832=ORIENTED_EDGE('',*,*,#5369,.T.);
#6833=ORIENTED_EDGE('',*,*,#5329,.T.);
#6834=ORIENTED_EDGE('',*,*,#5435,.T.);
#6835=ORIENTED_EDGE('',*,*,#5382,.F.);
#6836=ORIENTED_EDGE('',*,*,#5434,.F.);
#6837=ORIENTED_EDGE('',*,*,#5328,.T.);
#6838=ORIENTED_EDGE('',*,*,#5372,.T.);
#6839=ORIENTED_EDGE('',*,*,#5383,.F.);
#6840=ORIENTED_EDGE('',*,*,#5435,.F.);
#6841=ORIENTED_EDGE('',*,*,#5314,.F.);
#6842=ORIENTED_EDGE('',*,*,#5311,.F.);
#6843=ORIENTED_EDGE('',*,*,#5436,.F.);
#6844=ORIENTED_EDGE('',*,*,#5348,.F.);
#6845=ORIENTED_EDGE('',*,*,#5317,.T.);
#6846=ORIENTED_EDGE('',*,*,#5436,.T.);
#6847=ORIENTED_EDGE('',*,*,#5347,.T.);
#6848=ORIENTED_EDGE('',*,*,#5401,.T.);
#6849=ORIENTED_EDGE('',*,*,#5437,.T.);
#6850=ORIENTED_EDGE('',*,*,#5438,.T.);
#6851=ORIENTED_EDGE('',*,*,#5439,.F.);
#6852=ORIENTED_EDGE('',*,*,#5440,.T.);
#6853=ORIENTED_EDGE('',*,*,#5441,.T.);
#6854=ORIENTED_EDGE('',*,*,#5442,.T.);
#6855=ORIENTED_EDGE('',*,*,#5443,.F.);
#6856=ORIENTED_EDGE('',*,*,#5442,.F.);
#6857=ORIENTED_EDGE('',*,*,#5444,.F.);
#6858=ORIENTED_EDGE('',*,*,#5445,.T.);
#6859=ORIENTED_EDGE('',*,*,#5446,.F.);
#6860=ORIENTED_EDGE('',*,*,#5445,.F.);
#6861=ORIENTED_EDGE('',*,*,#5447,.T.);
#6862=ORIENTED_EDGE('',*,*,#5448,.T.);
#6863=ORIENTED_EDGE('',*,*,#5449,.T.);
#6864=ORIENTED_EDGE('',*,*,#5450,.F.);
#6865=ORIENTED_EDGE('',*,*,#5451,.T.);
#6866=ORIENTED_EDGE('',*,*,#5448,.F.);
#6867=ORIENTED_EDGE('',*,*,#5452,.T.);
#6868=ORIENTED_EDGE('',*,*,#5453,.T.);
#6869=ORIENTED_EDGE('',*,*,#5454,.T.);
#6870=ORIENTED_EDGE('',*,*,#5455,.F.);
#6871=ORIENTED_EDGE('',*,*,#5456,.T.);
#6872=ORIENTED_EDGE('',*,*,#5453,.F.);
#6873=ORIENTED_EDGE('',*,*,#5457,.T.);
#6874=ORIENTED_EDGE('',*,*,#5458,.T.);
#6875=ORIENTED_EDGE('',*,*,#5459,.T.);
#6876=ORIENTED_EDGE('',*,*,#5460,.F.);
#6877=ORIENTED_EDGE('',*,*,#5461,.T.);
#6878=ORIENTED_EDGE('',*,*,#5458,.F.);
#6879=ORIENTED_EDGE('',*,*,#5440,.F.);
#6880=ORIENTED_EDGE('',*,*,#5462,.F.);
#6881=ORIENTED_EDGE('',*,*,#5438,.F.);
#6882=ORIENTED_EDGE('',*,*,#5463,.T.);
#6883=ORIENTED_EDGE('',*,*,#5464,.T.);
#6884=ORIENTED_EDGE('',*,*,#5465,.F.);
#6885=ORIENTED_EDGE('',*,*,#5466,.F.);
#6886=ORIENTED_EDGE('',*,*,#5467,.T.);
#6887=ORIENTED_EDGE('',*,*,#5468,.F.);
#6888=ORIENTED_EDGE('',*,*,#5469,.T.);
#6889=ORIENTED_EDGE('',*,*,#5470,.T.);
#6890=ORIENTED_EDGE('',*,*,#5471,.F.);
#6891=ORIENTED_EDGE('',*,*,#5472,.F.);
#6892=ORIENTED_EDGE('',*,*,#5473,.F.);
#6893=ORIENTED_EDGE('',*,*,#5474,.T.);
#6894=ORIENTED_EDGE('',*,*,#5475,.T.);
#6895=ORIENTED_EDGE('',*,*,#5476,.T.);
#6896=ORIENTED_EDGE('',*,*,#5477,.F.);
#6897=ORIENTED_EDGE('',*,*,#5478,.F.);
#6898=ORIENTED_EDGE('',*,*,#5479,.T.);
#6899=ORIENTED_EDGE('',*,*,#5461,.F.);
#6900=ORIENTED_EDGE('',*,*,#5480,.F.);
#6901=ORIENTED_EDGE('',*,*,#5459,.F.);
#6902=ORIENTED_EDGE('',*,*,#5451,.F.);
#6903=ORIENTED_EDGE('',*,*,#5481,.F.);
#6904=ORIENTED_EDGE('',*,*,#5449,.F.);
#6905=ORIENTED_EDGE('',*,*,#5456,.F.);
#6906=ORIENTED_EDGE('',*,*,#5482,.F.);
#6907=ORIENTED_EDGE('',*,*,#5454,.F.);
#6908=ORIENTED_EDGE('',*,*,#5483,.T.);
#6909=ORIENTED_EDGE('',*,*,#5484,.F.);
#6910=ORIENTED_EDGE('',*,*,#5485,.F.);
#6911=ORIENTED_EDGE('',*,*,#5465,.T.);
#6912=ORIENTED_EDGE('',*,*,#5486,.T.);
#6913=ORIENTED_EDGE('',*,*,#5487,.F.);
#6914=ORIENTED_EDGE('',*,*,#5488,.F.);
#6915=ORIENTED_EDGE('',*,*,#5484,.T.);
#6916=ORIENTED_EDGE('',*,*,#5489,.T.);
#6917=ORIENTED_EDGE('',*,*,#5490,.F.);
#6918=ORIENTED_EDGE('',*,*,#5491,.F.);
#6919=ORIENTED_EDGE('',*,*,#5487,.T.);
#6920=ORIENTED_EDGE('',*,*,#5492,.T.);
#6921=ORIENTED_EDGE('',*,*,#5493,.F.);
#6922=ORIENTED_EDGE('',*,*,#5494,.F.);
#6923=ORIENTED_EDGE('',*,*,#5490,.T.);
#6924=ORIENTED_EDGE('',*,*,#5495,.T.);
#6925=ORIENTED_EDGE('',*,*,#5496,.F.);
#6926=ORIENTED_EDGE('',*,*,#5497,.F.);
#6927=ORIENTED_EDGE('',*,*,#5493,.T.);
#6928=ORIENTED_EDGE('',*,*,#5498,.T.);
#6929=ORIENTED_EDGE('',*,*,#5479,.F.);
#6930=ORIENTED_EDGE('',*,*,#5499,.F.);
#6931=ORIENTED_EDGE('',*,*,#5496,.T.);
#6932=ORIENTED_EDGE('',*,*,#5500,.T.);
#6933=ORIENTED_EDGE('',*,*,#5501,.F.);
#6934=ORIENTED_EDGE('',*,*,#5502,.F.);
#6935=ORIENTED_EDGE('',*,*,#5477,.T.);
#6936=ORIENTED_EDGE('',*,*,#5503,.T.);
#6937=ORIENTED_EDGE('',*,*,#5504,.F.);
#6938=ORIENTED_EDGE('',*,*,#5505,.F.);
#6939=ORIENTED_EDGE('',*,*,#5501,.T.);
#6940=ORIENTED_EDGE('',*,*,#5447,.F.);
#6941=ORIENTED_EDGE('',*,*,#5452,.F.);
#6942=ORIENTED_EDGE('',*,*,#5457,.F.);
#6943=ORIENTED_EDGE('',*,*,#5506,.T.);
#6944=ORIENTED_EDGE('',*,*,#5507,.F.);
#6945=ORIENTED_EDGE('',*,*,#5508,.F.);
#6946=ORIENTED_EDGE('',*,*,#5504,.T.);
#6947=ORIENTED_EDGE('',*,*,#5437,.F.);
#6948=ORIENTED_EDGE('',*,*,#5467,.F.);
#6949=ORIENTED_EDGE('',*,*,#5509,.F.);
#6950=ORIENTED_EDGE('',*,*,#5507,.T.);
#6951=ORIENTED_EDGE('',*,*,#5510,.T.);
#6952=ORIENTED_EDGE('',*,*,#5463,.F.);
#6953=ORIENTED_EDGE('',*,*,#5485,.T.);
#6954=ORIENTED_EDGE('',*,*,#5488,.T.);
#6955=ORIENTED_EDGE('',*,*,#5491,.T.);
#6956=ORIENTED_EDGE('',*,*,#5494,.T.);
#6957=ORIENTED_EDGE('',*,*,#5497,.T.);
#6958=ORIENTED_EDGE('',*,*,#5499,.T.);
#6959=ORIENTED_EDGE('',*,*,#5478,.T.);
#6960=ORIENTED_EDGE('',*,*,#5502,.T.);
#6961=ORIENTED_EDGE('',*,*,#5505,.T.);
#6962=ORIENTED_EDGE('',*,*,#5508,.T.);
#6963=ORIENTED_EDGE('',*,*,#5509,.T.);
#6964=ORIENTED_EDGE('',*,*,#5466,.T.);
#6965=ORIENTED_EDGE('',*,*,#5483,.F.);
#6966=ORIENTED_EDGE('',*,*,#5464,.F.);
#6967=ORIENTED_EDGE('',*,*,#5510,.F.);
#6968=ORIENTED_EDGE('',*,*,#5506,.F.);
#6969=ORIENTED_EDGE('',*,*,#5503,.F.);
#6970=ORIENTED_EDGE('',*,*,#5500,.F.);
#6971=ORIENTED_EDGE('',*,*,#5476,.F.);
#6972=ORIENTED_EDGE('',*,*,#5498,.F.);
#6973=ORIENTED_EDGE('',*,*,#5495,.F.);
#6974=ORIENTED_EDGE('',*,*,#5492,.F.);
#6975=ORIENTED_EDGE('',*,*,#5489,.F.);
#6976=ORIENTED_EDGE('',*,*,#5486,.F.);
#6977=ORIENTED_EDGE('',*,*,#5511,.T.);
#6978=ORIENTED_EDGE('',*,*,#5512,.F.);
#6979=ORIENTED_EDGE('',*,*,#5513,.F.);
#6980=ORIENTED_EDGE('',*,*,#5471,.T.);
#6981=ORIENTED_EDGE('',*,*,#5514,.T.);
#6982=ORIENTED_EDGE('',*,*,#5515,.F.);
#6983=ORIENTED_EDGE('',*,*,#5516,.F.);
#6984=ORIENTED_EDGE('',*,*,#5512,.T.);
#6985=ORIENTED_EDGE('',*,*,#5517,.T.);
#6986=ORIENTED_EDGE('',*,*,#5518,.F.);
#6987=ORIENTED_EDGE('',*,*,#5519,.F.);
#6988=ORIENTED_EDGE('',*,*,#5515,.T.);
#6989=ORIENTED_EDGE('',*,*,#5520,.T.);
#6990=ORIENTED_EDGE('',*,*,#5469,.F.);
#6991=ORIENTED_EDGE('',*,*,#5521,.F.);
#6992=ORIENTED_EDGE('',*,*,#5518,.T.);
#6993=ORIENTED_EDGE('',*,*,#5513,.T.);
#6994=ORIENTED_EDGE('',*,*,#5516,.T.);
#6995=ORIENTED_EDGE('',*,*,#5519,.T.);
#6996=ORIENTED_EDGE('',*,*,#5521,.T.);
#6997=ORIENTED_EDGE('',*,*,#5468,.T.);
#6998=ORIENTED_EDGE('',*,*,#5441,.F.);
#6999=ORIENTED_EDGE('',*,*,#5511,.F.);
#7000=ORIENTED_EDGE('',*,*,#5470,.F.);
#7001=ORIENTED_EDGE('',*,*,#5520,.F.);
#7002=ORIENTED_EDGE('',*,*,#5517,.F.);
#7003=ORIENTED_EDGE('',*,*,#5514,.F.);
#7004=ORIENTED_EDGE('',*,*,#5522,.T.);
#7005=ORIENTED_EDGE('',*,*,#5474,.F.);
#7006=ORIENTED_EDGE('',*,*,#5523,.F.);
#7007=ORIENTED_EDGE('',*,*,#5524,.T.);
#7008=ORIENTED_EDGE('',*,*,#5525,.T.);
#7009=ORIENTED_EDGE('',*,*,#5526,.F.);
#7010=ORIENTED_EDGE('',*,*,#5527,.F.);
#7011=ORIENTED_EDGE('',*,*,#5472,.T.);
#7012=ORIENTED_EDGE('',*,*,#5528,.T.);
#7013=ORIENTED_EDGE('',*,*,#5529,.F.);
#7014=ORIENTED_EDGE('',*,*,#5530,.F.);
#7015=ORIENTED_EDGE('',*,*,#5526,.T.);
#7016=ORIENTED_EDGE('',*,*,#5531,.T.);
#7017=ORIENTED_EDGE('',*,*,#5524,.F.);
#7018=ORIENTED_EDGE('',*,*,#5532,.F.);
#7019=ORIENTED_EDGE('',*,*,#5529,.T.);
#7020=ORIENTED_EDGE('',*,*,#5523,.T.);
#7021=ORIENTED_EDGE('',*,*,#5473,.T.);
#7022=ORIENTED_EDGE('',*,*,#5527,.T.);
#7023=ORIENTED_EDGE('',*,*,#5530,.T.);
#7024=ORIENTED_EDGE('',*,*,#5532,.T.);
#7025=ORIENTED_EDGE('',*,*,#5444,.T.);
#7026=ORIENTED_EDGE('',*,*,#5522,.F.);
#7027=ORIENTED_EDGE('',*,*,#5531,.F.);
#7028=ORIENTED_EDGE('',*,*,#5528,.F.);
#7029=ORIENTED_EDGE('',*,*,#5525,.F.);
#7030=ORIENTED_EDGE('',*,*,#5475,.F.);
#7031=ORIENTED_EDGE('',*,*,#5480,.T.);
#7032=ORIENTED_EDGE('',*,*,#5460,.T.);
#7033=ORIENTED_EDGE('',*,*,#5482,.T.);
#7034=ORIENTED_EDGE('',*,*,#5455,.T.);
#7035=ORIENTED_EDGE('',*,*,#5481,.T.);
#7036=ORIENTED_EDGE('',*,*,#5450,.T.);
#7037=ORIENTED_EDGE('',*,*,#5446,.T.);
#7038=ORIENTED_EDGE('',*,*,#5443,.T.);
#7039=ORIENTED_EDGE('',*,*,#5462,.T.);
#7040=ORIENTED_EDGE('',*,*,#5439,.T.);
#7041=ORIENTED_EDGE('',*,*,#5533,.T.);
#7042=ORIENTED_EDGE('',*,*,#5534,.T.);
#7043=ORIENTED_EDGE('',*,*,#5535,.F.);
#7044=ORIENTED_EDGE('',*,*,#5536,.T.);
#7045=ORIENTED_EDGE('',*,*,#5537,.F.);
#7046=ORIENTED_EDGE('',*,*,#5534,.F.);
#7047=ORIENTED_EDGE('',*,*,#5538,.T.);
#7048=ORIENTED_EDGE('',*,*,#5539,.T.);
#7049=ORIENTED_EDGE('',*,*,#5540,.F.);
#7050=ORIENTED_EDGE('',*,*,#5541,.T.);
#7051=ORIENTED_EDGE('',*,*,#5542,.F.);
#7052=ORIENTED_EDGE('',*,*,#5539,.F.);
#7053=ORIENTED_EDGE('',*,*,#5543,.T.);
#7054=ORIENTED_EDGE('',*,*,#5544,.T.);
#7055=ORIENTED_EDGE('',*,*,#5545,.F.);
#7056=ORIENTED_EDGE('',*,*,#5546,.T.);
#7057=ORIENTED_EDGE('',*,*,#5547,.F.);
#7058=ORIENTED_EDGE('',*,*,#5544,.F.);
#7059=ORIENTED_EDGE('',*,*,#5548,.T.);
#7060=ORIENTED_EDGE('',*,*,#5549,.T.);
#7061=ORIENTED_EDGE('',*,*,#5550,.F.);
#7062=ORIENTED_EDGE('',*,*,#5549,.F.);
#7063=ORIENTED_EDGE('',*,*,#5551,.T.);
#7064=ORIENTED_EDGE('',*,*,#5552,.T.);
#7065=ORIENTED_EDGE('',*,*,#5553,.F.);
#7066=ORIENTED_EDGE('',*,*,#5552,.F.);
#7067=ORIENTED_EDGE('',*,*,#5554,.T.);
#7068=ORIENTED_EDGE('',*,*,#5555,.T.);
#7069=ORIENTED_EDGE('',*,*,#5556,.T.);
#7070=ORIENTED_EDGE('',*,*,#5555,.F.);
#7071=ORIENTED_EDGE('',*,*,#5557,.F.);
#7072=ORIENTED_EDGE('',*,*,#5558,.F.);
#7073=ORIENTED_EDGE('',*,*,#5559,.T.);
#7074=ORIENTED_EDGE('',*,*,#5560,.T.);
#7075=ORIENTED_EDGE('',*,*,#5561,.F.);
#7076=ORIENTED_EDGE('',*,*,#5562,.T.);
#7077=ORIENTED_EDGE('',*,*,#5563,.T.);
#7078=ORIENTED_EDGE('',*,*,#5564,.T.);
#7079=ORIENTED_EDGE('',*,*,#5565,.F.);
#7080=ORIENTED_EDGE('',*,*,#5566,.T.);
#7081=ORIENTED_EDGE('',*,*,#5567,.T.);
#7082=ORIENTED_EDGE('',*,*,#5568,.T.);
#7083=ORIENTED_EDGE('',*,*,#5569,.F.);
#7084=ORIENTED_EDGE('',*,*,#5570,.F.);
#7085=ORIENTED_EDGE('',*,*,#5571,.T.);
#7086=ORIENTED_EDGE('',*,*,#5572,.F.);
#7087=ORIENTED_EDGE('',*,*,#5573,.F.);
#7088=ORIENTED_EDGE('',*,*,#5574,.F.);
#7089=ORIENTED_EDGE('',*,*,#5575,.F.);
#7090=ORIENTED_EDGE('',*,*,#5576,.F.);
#7091=ORIENTED_EDGE('',*,*,#5577,.F.);
#7092=ORIENTED_EDGE('',*,*,#5578,.F.);
#7093=ORIENTED_EDGE('',*,*,#5579,.F.);
#7094=ORIENTED_EDGE('',*,*,#5580,.F.);
#7095=ORIENTED_EDGE('',*,*,#5581,.T.);
#7096=ORIENTED_EDGE('',*,*,#5582,.T.);
#7097=ORIENTED_EDGE('',*,*,#5583,.F.);
#7098=ORIENTED_EDGE('',*,*,#5584,.F.);
#7099=ORIENTED_EDGE('',*,*,#5585,.F.);
#7100=ORIENTED_EDGE('',*,*,#5586,.F.);
#7101=ORIENTED_EDGE('',*,*,#5587,.F.);
#7102=ORIENTED_EDGE('',*,*,#5588,.F.);
#7103=ORIENTED_EDGE('',*,*,#5589,.F.);
#7104=ORIENTED_EDGE('',*,*,#5590,.F.);
#7105=ORIENTED_EDGE('',*,*,#5591,.F.);
#7106=ORIENTED_EDGE('',*,*,#5592,.T.);
#7107=ORIENTED_EDGE('',*,*,#5583,.T.);
#7108=ORIENTED_EDGE('',*,*,#5593,.T.);
#7109=ORIENTED_EDGE('',*,*,#5594,.T.);
#7110=ORIENTED_EDGE('',*,*,#5595,.T.);
#7111=ORIENTED_EDGE('',*,*,#5591,.T.);
#7112=ORIENTED_EDGE('',*,*,#5596,.F.);
#7113=ORIENTED_EDGE('',*,*,#5597,.F.);
#7114=ORIENTED_EDGE('',*,*,#5598,.F.);
#7115=ORIENTED_EDGE('',*,*,#5570,.T.);
#7116=ORIENTED_EDGE('',*,*,#5599,.T.);
#7117=ORIENTED_EDGE('',*,*,#5600,.T.);
#7118=ORIENTED_EDGE('',*,*,#5601,.F.);
#7119=ORIENTED_EDGE('',*,*,#5602,.T.);
#7120=ORIENTED_EDGE('',*,*,#5603,.T.);
#7121=ORIENTED_EDGE('',*,*,#5578,.T.);
#7122=ORIENTED_EDGE('',*,*,#5604,.T.);
#7123=ORIENTED_EDGE('',*,*,#5605,.F.);
#7124=ORIENTED_EDGE('',*,*,#5606,.T.);
#7125=ORIENTED_EDGE('',*,*,#5572,.T.);
#7126=ORIENTED_EDGE('',*,*,#5607,.F.);
#7127=ORIENTED_EDGE('',*,*,#5576,.T.);
#7128=ORIENTED_EDGE('',*,*,#5608,.T.);
#7129=ORIENTED_EDGE('',*,*,#5609,.F.);
#7130=ORIENTED_EDGE('',*,*,#5610,.T.);
#7131=ORIENTED_EDGE('',*,*,#5600,.F.);
#7132=ORIENTED_EDGE('',*,*,#5611,.T.);
#7133=ORIENTED_EDGE('',*,*,#5612,.T.);
#7134=ORIENTED_EDGE('',*,*,#5613,.F.);
#7135=ORIENTED_EDGE('',*,*,#5614,.T.);
#7136=ORIENTED_EDGE('',*,*,#5615,.T.);
#7137=ORIENTED_EDGE('',*,*,#5602,.F.);
#7138=ORIENTED_EDGE('',*,*,#5616,.T.);
#7139=ORIENTED_EDGE('',*,*,#5617,.F.);
#7140=ORIENTED_EDGE('',*,*,#5618,.T.);
#7141=ORIENTED_EDGE('',*,*,#5619,.T.);
#7142=ORIENTED_EDGE('',*,*,#5620,.F.);
#7143=ORIENTED_EDGE('',*,*,#5621,.T.);
#7144=ORIENTED_EDGE('',*,*,#5622,.T.);
#7145=ORIENTED_EDGE('',*,*,#5623,.F.);
#7146=ORIENTED_EDGE('',*,*,#5624,.T.);
#7147=ORIENTED_EDGE('',*,*,#5625,.F.);
#7148=ORIENTED_EDGE('',*,*,#5626,.T.);
#7149=ORIENTED_EDGE('',*,*,#5605,.T.);
#7150=ORIENTED_EDGE('',*,*,#5627,.F.);
#7151=ORIENTED_EDGE('',*,*,#5609,.T.);
#7152=ORIENTED_EDGE('',*,*,#5628,.T.);
#7153=ORIENTED_EDGE('',*,*,#5629,.F.);
#7154=ORIENTED_EDGE('',*,*,#5630,.T.);
#7155=ORIENTED_EDGE('',*,*,#5588,.T.);
#7156=ORIENTED_EDGE('',*,*,#5631,.F.);
#7157=ORIENTED_EDGE('',*,*,#5632,.F.);
#7158=ORIENTED_EDGE('',*,*,#5633,.T.);
#7159=ORIENTED_EDGE('',*,*,#5546,.F.);
#7160=ORIENTED_EDGE('',*,*,#5634,.F.);
#7161=ORIENTED_EDGE('',*,*,#5536,.F.);
#7162=ORIENTED_EDGE('',*,*,#5635,.F.);
#7163=ORIENTED_EDGE('',*,*,#5541,.F.);
#7164=ORIENTED_EDGE('',*,*,#5636,.F.);
#7165=ORIENTED_EDGE('',*,*,#5637,.F.);
#7166=ORIENTED_EDGE('',*,*,#5638,.T.);
#7167=ORIENTED_EDGE('',*,*,#5639,.F.);
#7168=ORIENTED_EDGE('',*,*,#5561,.T.);
#7169=ORIENTED_EDGE('',*,*,#5640,.T.);
#7170=ORIENTED_EDGE('',*,*,#5596,.T.);
#7171=ORIENTED_EDGE('',*,*,#5590,.T.);
#7172=ORIENTED_EDGE('',*,*,#5641,.F.);
#7173=ORIENTED_EDGE('',*,*,#5533,.F.);
#7174=ORIENTED_EDGE('',*,*,#5538,.F.);
#7175=ORIENTED_EDGE('',*,*,#5543,.F.);
#7176=ORIENTED_EDGE('',*,*,#5589,.T.);
#7177=ORIENTED_EDGE('',*,*,#5633,.F.);
#7178=ORIENTED_EDGE('',*,*,#5642,.F.);
#7179=ORIENTED_EDGE('',*,*,#5641,.T.);
#7180=ORIENTED_EDGE('',*,*,#5587,.T.);
#7181=ORIENTED_EDGE('',*,*,#5643,.F.);
#7182=ORIENTED_EDGE('',*,*,#5644,.F.);
#7183=ORIENTED_EDGE('',*,*,#5631,.T.);
#7184=ORIENTED_EDGE('',*,*,#5586,.T.);
#7185=ORIENTED_EDGE('',*,*,#5645,.F.);
#7186=ORIENTED_EDGE('',*,*,#5646,.F.);
#7187=ORIENTED_EDGE('',*,*,#5643,.T.);
#7188=ORIENTED_EDGE('',*,*,#5585,.T.);
#7189=ORIENTED_EDGE('',*,*,#5647,.F.);
#7190=ORIENTED_EDGE('',*,*,#5648,.F.);
#7191=ORIENTED_EDGE('',*,*,#5645,.T.);
#7192=ORIENTED_EDGE('',*,*,#5584,.T.);
#7193=ORIENTED_EDGE('',*,*,#5598,.T.);
#7194=ORIENTED_EDGE('',*,*,#5649,.F.);
#7195=ORIENTED_EDGE('',*,*,#5567,.F.);
#7196=ORIENTED_EDGE('',*,*,#5650,.T.);
#7197=ORIENTED_EDGE('',*,*,#5651,.T.);
#7198=ORIENTED_EDGE('',*,*,#5652,.F.);
#7199=ORIENTED_EDGE('',*,*,#5647,.T.);
#7200=ORIENTED_EDGE('',*,*,#5652,.T.);
#7201=ORIENTED_EDGE('',*,*,#5653,.T.);
#7202=ORIENTED_EDGE('',*,*,#5637,.T.);
#7203=ORIENTED_EDGE('',*,*,#5642,.T.);
#7204=ORIENTED_EDGE('',*,*,#5632,.T.);
#7205=ORIENTED_EDGE('',*,*,#5644,.T.);
#7206=ORIENTED_EDGE('',*,*,#5646,.T.);
#7207=ORIENTED_EDGE('',*,*,#5648,.T.);
#7208=ORIENTED_EDGE('',*,*,#5597,.T.);
#7209=ORIENTED_EDGE('',*,*,#5640,.F.);
#7210=ORIENTED_EDGE('',*,*,#5560,.F.);
#7211=ORIENTED_EDGE('',*,*,#5654,.F.);
#7212=ORIENTED_EDGE('',*,*,#5655,.F.);
#7213=ORIENTED_EDGE('',*,*,#5656,.F.);
#7214=ORIENTED_EDGE('',*,*,#5657,.F.);
#7215=ORIENTED_EDGE('',*,*,#5658,.F.);
#7216=ORIENTED_EDGE('',*,*,#5568,.F.);
#7217=ORIENTED_EDGE('',*,*,#5649,.T.);
#7218=ORIENTED_EDGE('',*,*,#5556,.F.);
#7219=ORIENTED_EDGE('',*,*,#5653,.F.);
#7220=ORIENTED_EDGE('',*,*,#5651,.F.);
#7221=ORIENTED_EDGE('',*,*,#5659,.F.);
#7222=ORIENTED_EDGE('',*,*,#5638,.F.);
#7223=ORIENTED_EDGE('',*,*,#5659,.T.);
#7224=ORIENTED_EDGE('',*,*,#5650,.F.);
#7225=ORIENTED_EDGE('',*,*,#5566,.F.);
#7226=ORIENTED_EDGE('',*,*,#5660,.T.);
#7227=ORIENTED_EDGE('',*,*,#5661,.T.);
#7228=ORIENTED_EDGE('',*,*,#5662,.T.);
#7229=ORIENTED_EDGE('',*,*,#5663,.T.);
#7230=ORIENTED_EDGE('',*,*,#5664,.T.);
#7231=ORIENTED_EDGE('',*,*,#5562,.F.);
#7232=ORIENTED_EDGE('',*,*,#5639,.T.);
#7233=ORIENTED_EDGE('',*,*,#5665,.T.);
#7234=ORIENTED_EDGE('',*,*,#5666,.F.);
#7235=ORIENTED_EDGE('',*,*,#5660,.F.);
#7236=ORIENTED_EDGE('',*,*,#5565,.T.);
#7237=ORIENTED_EDGE('',*,*,#5667,.T.);
#7238=ORIENTED_EDGE('',*,*,#5668,.F.);
#7239=ORIENTED_EDGE('',*,*,#5661,.F.);
#7240=ORIENTED_EDGE('',*,*,#5666,.T.);
#7241=ORIENTED_EDGE('',*,*,#5669,.T.);
#7242=ORIENTED_EDGE('',*,*,#5670,.F.);
#7243=ORIENTED_EDGE('',*,*,#5662,.F.);
#7244=ORIENTED_EDGE('',*,*,#5668,.T.);
#7245=ORIENTED_EDGE('',*,*,#5671,.T.);
#7246=ORIENTED_EDGE('',*,*,#5672,.F.);
#7247=ORIENTED_EDGE('',*,*,#5663,.F.);
#7248=ORIENTED_EDGE('',*,*,#5670,.T.);
#7249=ORIENTED_EDGE('',*,*,#5673,.T.);
#7250=ORIENTED_EDGE('',*,*,#5563,.F.);
#7251=ORIENTED_EDGE('',*,*,#5664,.F.);
#7252=ORIENTED_EDGE('',*,*,#5672,.T.);
#7253=ORIENTED_EDGE('',*,*,#5665,.F.);
#7254=ORIENTED_EDGE('',*,*,#5564,.F.);
#7255=ORIENTED_EDGE('',*,*,#5673,.F.);
#7256=ORIENTED_EDGE('',*,*,#5671,.F.);
#7257=ORIENTED_EDGE('',*,*,#5669,.F.);
#7258=ORIENTED_EDGE('',*,*,#5667,.F.);
#7259=ORIENTED_EDGE('',*,*,#5550,.T.);
#7260=ORIENTED_EDGE('',*,*,#5553,.T.);
#7261=ORIENTED_EDGE('',*,*,#5658,.T.);
#7262=ORIENTED_EDGE('',*,*,#5674,.F.);
#7263=ORIENTED_EDGE('',*,*,#5675,.F.);
#7264=ORIENTED_EDGE('',*,*,#5557,.T.);
#7265=ORIENTED_EDGE('',*,*,#5657,.T.);
#7266=ORIENTED_EDGE('',*,*,#5676,.F.);
#7267=ORIENTED_EDGE('',*,*,#5677,.F.);
#7268=ORIENTED_EDGE('',*,*,#5674,.T.);
#7269=ORIENTED_EDGE('',*,*,#5656,.T.);
#7270=ORIENTED_EDGE('',*,*,#5678,.F.);
#7271=ORIENTED_EDGE('',*,*,#5679,.F.);
#7272=ORIENTED_EDGE('',*,*,#5676,.T.);
#7273=ORIENTED_EDGE('',*,*,#5655,.T.);
#7274=ORIENTED_EDGE('',*,*,#5680,.F.);
#7275=ORIENTED_EDGE('',*,*,#5681,.F.);
#7276=ORIENTED_EDGE('',*,*,#5678,.T.);
#7277=ORIENTED_EDGE('',*,*,#5654,.T.);
#7278=ORIENTED_EDGE('',*,*,#5559,.F.);
#7279=ORIENTED_EDGE('',*,*,#5682,.F.);
#7280=ORIENTED_EDGE('',*,*,#5680,.T.);
#7281=ORIENTED_EDGE('',*,*,#5675,.T.);
#7282=ORIENTED_EDGE('',*,*,#5677,.T.);
#7283=ORIENTED_EDGE('',*,*,#5679,.T.);
#7284=ORIENTED_EDGE('',*,*,#5681,.T.);
#7285=ORIENTED_EDGE('',*,*,#5682,.T.);
#7286=ORIENTED_EDGE('',*,*,#5558,.T.);
#7287=ORIENTED_EDGE('',*,*,#5554,.F.);
#7288=ORIENTED_EDGE('',*,*,#5577,.T.);
#7289=ORIENTED_EDGE('',*,*,#5610,.F.);
#7290=ORIENTED_EDGE('',*,*,#5630,.F.);
#7291=ORIENTED_EDGE('',*,*,#5683,.F.);
#7292=ORIENTED_EDGE('',*,*,#5624,.F.);
#7293=ORIENTED_EDGE('',*,*,#5684,.F.);
#7294=ORIENTED_EDGE('',*,*,#5616,.F.);
#7295=ORIENTED_EDGE('',*,*,#5604,.F.);
#7296=ORIENTED_EDGE('',*,*,#5601,.T.);
#7297=ORIENTED_EDGE('',*,*,#5613,.T.);
#7298=ORIENTED_EDGE('',*,*,#5685,.T.);
#7299=ORIENTED_EDGE('',*,*,#5620,.T.);
#7300=ORIENTED_EDGE('',*,*,#5686,.T.);
#7301=ORIENTED_EDGE('',*,*,#5627,.T.);
#7302=ORIENTED_EDGE('',*,*,#5607,.T.);
#7303=ORIENTED_EDGE('',*,*,#5571,.F.);
#7304=ORIENTED_EDGE('',*,*,#5687,.F.);
#7305=ORIENTED_EDGE('',*,*,#5617,.T.);
#7306=ORIENTED_EDGE('',*,*,#5685,.F.);
#7307=ORIENTED_EDGE('',*,*,#5612,.F.);
#7308=ORIENTED_EDGE('',*,*,#5688,.F.);
#7309=ORIENTED_EDGE('',*,*,#5580,.T.);
#7310=ORIENTED_EDGE('',*,*,#5689,.T.);
#7311=ORIENTED_EDGE('',*,*,#5614,.F.);
#7312=ORIENTED_EDGE('',*,*,#5684,.T.);
#7313=ORIENTED_EDGE('',*,*,#5623,.T.);
#7314=ORIENTED_EDGE('',*,*,#5690,.T.);
#7315=ORIENTED_EDGE('',*,*,#5691,.F.);
#7316=ORIENTED_EDGE('',*,*,#5592,.F.);
#7317=ORIENTED_EDGE('',*,*,#5595,.F.);
#7318=ORIENTED_EDGE('',*,*,#5692,.T.);
#7319=ORIENTED_EDGE('',*,*,#5625,.T.);
#7320=ORIENTED_EDGE('',*,*,#5686,.F.);
#7321=ORIENTED_EDGE('',*,*,#5619,.F.);
#7322=ORIENTED_EDGE('',*,*,#5693,.T.);
#7323=ORIENTED_EDGE('',*,*,#5593,.F.);
#7324=ORIENTED_EDGE('',*,*,#5582,.F.);
#7325=ORIENTED_EDGE('',*,*,#5694,.F.);
#7326=ORIENTED_EDGE('',*,*,#5695,.F.);
#7327=ORIENTED_EDGE('',*,*,#5621,.F.);
#7328=ORIENTED_EDGE('',*,*,#5683,.T.);
#7329=ORIENTED_EDGE('',*,*,#5629,.T.);
#7330=ORIENTED_EDGE('',*,*,#5696,.F.);
#7331=ORIENTED_EDGE('',*,*,#5574,.T.);
#7332=ORIENTED_EDGE('',*,*,#5551,.F.);
#7333=ORIENTED_EDGE('',*,*,#5548,.F.);
#7334=ORIENTED_EDGE('',*,*,#5634,.T.);
#7335=ORIENTED_EDGE('',*,*,#5545,.T.);
#7336=ORIENTED_EDGE('',*,*,#5547,.T.);
#7337=ORIENTED_EDGE('',*,*,#5636,.T.);
#7338=ORIENTED_EDGE('',*,*,#5540,.T.);
#7339=ORIENTED_EDGE('',*,*,#5542,.T.);
#7340=ORIENTED_EDGE('',*,*,#5635,.T.);
#7341=ORIENTED_EDGE('',*,*,#5535,.T.);
#7342=ORIENTED_EDGE('',*,*,#5537,.T.);
#7343=ORIENTED_EDGE('',*,*,#5573,.T.);
#7344=ORIENTED_EDGE('',*,*,#5606,.F.);
#7345=ORIENTED_EDGE('',*,*,#5626,.F.);
#7346=ORIENTED_EDGE('',*,*,#5692,.F.);
#7347=ORIENTED_EDGE('',*,*,#5575,.T.);
#7348=ORIENTED_EDGE('',*,*,#5696,.T.);
#7349=ORIENTED_EDGE('',*,*,#5628,.F.);
#7350=ORIENTED_EDGE('',*,*,#5608,.F.);
#7351=ORIENTED_EDGE('',*,*,#5695,.T.);
#7352=ORIENTED_EDGE('',*,*,#5697,.F.);
#7353=ORIENTED_EDGE('',*,*,#5690,.F.);
#7354=ORIENTED_EDGE('',*,*,#5622,.F.);
#7355=ORIENTED_EDGE('',*,*,#5693,.F.);
#7356=ORIENTED_EDGE('',*,*,#5618,.F.);
#7357=ORIENTED_EDGE('',*,*,#5687,.T.);
#7358=ORIENTED_EDGE('',*,*,#5594,.F.);
#7359=ORIENTED_EDGE('',*,*,#5691,.T.);
#7360=ORIENTED_EDGE('',*,*,#5697,.T.);
#7361=ORIENTED_EDGE('',*,*,#5694,.T.);
#7362=ORIENTED_EDGE('',*,*,#5581,.F.);
#7363=ORIENTED_EDGE('',*,*,#5569,.T.);
#7364=ORIENTED_EDGE('',*,*,#5688,.T.);
#7365=ORIENTED_EDGE('',*,*,#5611,.F.);
#7366=ORIENTED_EDGE('',*,*,#5599,.F.);
#7367=ORIENTED_EDGE('',*,*,#5579,.T.);
#7368=ORIENTED_EDGE('',*,*,#5603,.F.);
#7369=ORIENTED_EDGE('',*,*,#5615,.F.);
#7370=ORIENTED_EDGE('',*,*,#5689,.F.);
#7371=ORIENTED_EDGE('',*,*,#5698,.T.);
#7372=ORIENTED_EDGE('',*,*,#5699,.T.);
#7373=ORIENTED_EDGE('',*,*,#5700,.F.);
#7374=ORIENTED_EDGE('',*,*,#5699,.F.);
#7375=ORIENTED_EDGE('',*,*,#5701,.T.);
#7376=ORIENTED_EDGE('',*,*,#5702,.T.);
#7377=ORIENTED_EDGE('',*,*,#5703,.F.);
#7378=ORIENTED_EDGE('',*,*,#5702,.F.);
#7379=ORIENTED_EDGE('',*,*,#5704,.T.);
#7380=ORIENTED_EDGE('',*,*,#5705,.T.);
#7381=ORIENTED_EDGE('',*,*,#5706,.F.);
#7382=ORIENTED_EDGE('',*,*,#5705,.F.);
#7383=ORIENTED_EDGE('',*,*,#5707,.T.);
#7384=ORIENTED_EDGE('',*,*,#5708,.T.);
#7385=ORIENTED_EDGE('',*,*,#5709,.F.);
#7386=ORIENTED_EDGE('',*,*,#5708,.F.);
#7387=ORIENTED_EDGE('',*,*,#5710,.T.);
#7388=ORIENTED_EDGE('',*,*,#5711,.T.);
#7389=ORIENTED_EDGE('',*,*,#5712,.F.);
#7390=ORIENTED_EDGE('',*,*,#5711,.F.);
#7391=ORIENTED_EDGE('',*,*,#5713,.F.);
#7392=ORIENTED_EDGE('',*,*,#5714,.F.);
#7393=ORIENTED_EDGE('',*,*,#5715,.T.);
#7394=ORIENTED_EDGE('',*,*,#5716,.T.);
#7395=ORIENTED_EDGE('',*,*,#5717,.F.);
#7396=ORIENTED_EDGE('',*,*,#5718,.T.);
#7397=ORIENTED_EDGE('',*,*,#5719,.F.);
#7398=ORIENTED_EDGE('',*,*,#5720,.F.);
#7399=ORIENTED_EDGE('',*,*,#5721,.T.);
#7400=ORIENTED_EDGE('',*,*,#5722,.F.);
#7401=ORIENTED_EDGE('',*,*,#5723,.F.);
#7402=ORIENTED_EDGE('',*,*,#5719,.T.);
#7403=ORIENTED_EDGE('',*,*,#5724,.T.);
#7404=ORIENTED_EDGE('',*,*,#5725,.F.);
#7405=ORIENTED_EDGE('',*,*,#5726,.F.);
#7406=ORIENTED_EDGE('',*,*,#5722,.T.);
#7407=ORIENTED_EDGE('',*,*,#5727,.T.);
#7408=ORIENTED_EDGE('',*,*,#5728,.F.);
#7409=ORIENTED_EDGE('',*,*,#5729,.F.);
#7410=ORIENTED_EDGE('',*,*,#5725,.T.);
#7411=ORIENTED_EDGE('',*,*,#5730,.T.);
#7412=ORIENTED_EDGE('',*,*,#5731,.F.);
#7413=ORIENTED_EDGE('',*,*,#5732,.F.);
#7414=ORIENTED_EDGE('',*,*,#5728,.T.);
#7415=ORIENTED_EDGE('',*,*,#5733,.T.);
#7416=ORIENTED_EDGE('',*,*,#5715,.F.);
#7417=ORIENTED_EDGE('',*,*,#5734,.F.);
#7418=ORIENTED_EDGE('',*,*,#5731,.T.);
#7419=ORIENTED_EDGE('',*,*,#5714,.T.);
#7420=ORIENTED_EDGE('',*,*,#5735,.T.);
#7421=ORIENTED_EDGE('',*,*,#5736,.T.);
#7422=ORIENTED_EDGE('',*,*,#5737,.F.);
#7423=ORIENTED_EDGE('',*,*,#5720,.T.);
#7424=ORIENTED_EDGE('',*,*,#5723,.T.);
#7425=ORIENTED_EDGE('',*,*,#5726,.T.);
#7426=ORIENTED_EDGE('',*,*,#5729,.T.);
#7427=ORIENTED_EDGE('',*,*,#5732,.T.);
#7428=ORIENTED_EDGE('',*,*,#5734,.T.);
#7429=ORIENTED_EDGE('',*,*,#5704,.F.);
#7430=ORIENTED_EDGE('',*,*,#5707,.F.);
#7431=ORIENTED_EDGE('',*,*,#5718,.F.);
#7432=ORIENTED_EDGE('',*,*,#5738,.T.);
#7433=ORIENTED_EDGE('',*,*,#5739,.T.);
#7434=ORIENTED_EDGE('',*,*,#5740,.F.);
#7435=ORIENTED_EDGE('',*,*,#5716,.F.);
#7436=ORIENTED_EDGE('',*,*,#5733,.F.);
#7437=ORIENTED_EDGE('',*,*,#5730,.F.);
#7438=ORIENTED_EDGE('',*,*,#5727,.F.);
#7439=ORIENTED_EDGE('',*,*,#5724,.F.);
#7440=ORIENTED_EDGE('',*,*,#5721,.F.);
#7441=ORIENTED_EDGE('',*,*,#5712,.T.);
#7442=ORIENTED_EDGE('',*,*,#5735,.F.);
#7443=ORIENTED_EDGE('',*,*,#5713,.T.);
#7444=ORIENTED_EDGE('',*,*,#5740,.T.);
#7445=ORIENTED_EDGE('',*,*,#5741,.T.);
#7446=ORIENTED_EDGE('',*,*,#5738,.F.);
#7447=ORIENTED_EDGE('',*,*,#5717,.T.);
#7448=ORIENTED_EDGE('',*,*,#5737,.T.);
#7449=ORIENTED_EDGE('',*,*,#5742,.T.);
#7450=ORIENTED_EDGE('',*,*,#5741,.F.);
#7451=ORIENTED_EDGE('',*,*,#5739,.F.);
#7452=ORIENTED_EDGE('',*,*,#5742,.F.);
#7453=ORIENTED_EDGE('',*,*,#5736,.F.);
#7454=ORIENTED_EDGE('',*,*,#5700,.T.);
#7455=ORIENTED_EDGE('',*,*,#5703,.T.);
#7456=ORIENTED_EDGE('',*,*,#5710,.F.);
#7457=ORIENTED_EDGE('',*,*,#5709,.T.);
#7458=ORIENTED_EDGE('',*,*,#5706,.T.);
#7459=ORIENTED_EDGE('',*,*,#5701,.F.);
#7460=ORIENTED_EDGE('',*,*,#5698,.F.);
#7461=ORIENTED_EDGE('',*,*,#5743,.T.);
#7462=ORIENTED_EDGE('',*,*,#5744,.F.);
#7463=ORIENTED_EDGE('',*,*,#5745,.F.);
#7464=ORIENTED_EDGE('',*,*,#5746,.T.);
#7465=ORIENTED_EDGE('',*,*,#5747,.T.);
#7466=ORIENTED_EDGE('',*,*,#5748,.F.);
#7467=ORIENTED_EDGE('',*,*,#5749,.F.);
#7468=ORIENTED_EDGE('',*,*,#5744,.T.);
#7469=ORIENTED_EDGE('',*,*,#5750,.T.);
#7470=ORIENTED_EDGE('',*,*,#5751,.F.);
#7471=ORIENTED_EDGE('',*,*,#5752,.F.);
#7472=ORIENTED_EDGE('',*,*,#5748,.T.);
#7473=ORIENTED_EDGE('',*,*,#5753,.T.);
#7474=ORIENTED_EDGE('',*,*,#5746,.F.);
#7475=ORIENTED_EDGE('',*,*,#5754,.F.);
#7476=ORIENTED_EDGE('',*,*,#5751,.T.);
#7477=ORIENTED_EDGE('',*,*,#5745,.T.);
#7478=ORIENTED_EDGE('',*,*,#5749,.T.);
#7479=ORIENTED_EDGE('',*,*,#5752,.T.);
#7480=ORIENTED_EDGE('',*,*,#5754,.T.);
#7481=ORIENTED_EDGE('',*,*,#5743,.F.);
#7482=ORIENTED_EDGE('',*,*,#5753,.F.);
#7483=ORIENTED_EDGE('',*,*,#5750,.F.);
#7484=ORIENTED_EDGE('',*,*,#5747,.F.);
#7485=ORIENTED_EDGE('',*,*,#5755,.T.);
#7486=ORIENTED_EDGE('',*,*,#5756,.F.);
#7487=ORIENTED_EDGE('',*,*,#5757,.F.);
#7488=ORIENTED_EDGE('',*,*,#5758,.T.);
#7489=ORIENTED_EDGE('',*,*,#5759,.T.);
#7490=ORIENTED_EDGE('',*,*,#5760,.F.);
#7491=ORIENTED_EDGE('',*,*,#5761,.F.);
#7492=ORIENTED_EDGE('',*,*,#5756,.T.);
#7493=ORIENTED_EDGE('',*,*,#5762,.T.);
#7494=ORIENTED_EDGE('',*,*,#5763,.F.);
#7495=ORIENTED_EDGE('',*,*,#5764,.F.);
#7496=ORIENTED_EDGE('',*,*,#5760,.T.);
#7497=ORIENTED_EDGE('',*,*,#5765,.T.);
#7498=ORIENTED_EDGE('',*,*,#5758,.F.);
#7499=ORIENTED_EDGE('',*,*,#5766,.F.);
#7500=ORIENTED_EDGE('',*,*,#5763,.T.);
#7501=ORIENTED_EDGE('',*,*,#5757,.T.);
#7502=ORIENTED_EDGE('',*,*,#5761,.T.);
#7503=ORIENTED_EDGE('',*,*,#5764,.T.);
#7504=ORIENTED_EDGE('',*,*,#5766,.T.);
#7505=ORIENTED_EDGE('',*,*,#5755,.F.);
#7506=ORIENTED_EDGE('',*,*,#5765,.F.);
#7507=ORIENTED_EDGE('',*,*,#5762,.F.);
#7508=ORIENTED_EDGE('',*,*,#5759,.F.);
#7509=ORIENTED_EDGE('',*,*,#5767,.T.);
#7510=ORIENTED_EDGE('',*,*,#5768,.T.);
#7511=ORIENTED_EDGE('',*,*,#5769,.F.);
#7512=ORIENTED_EDGE('',*,*,#5768,.F.);
#7513=ORIENTED_EDGE('',*,*,#5770,.T.);
#7514=ORIENTED_EDGE('',*,*,#5771,.T.);
#7515=ORIENTED_EDGE('',*,*,#5772,.F.);
#7516=ORIENTED_EDGE('',*,*,#5771,.F.);
#7517=ORIENTED_EDGE('',*,*,#5773,.T.);
#7518=ORIENTED_EDGE('',*,*,#5774,.T.);
#7519=ORIENTED_EDGE('',*,*,#5775,.F.);
#7520=ORIENTED_EDGE('',*,*,#5774,.F.);
#7521=ORIENTED_EDGE('',*,*,#5776,.T.);
#7522=ORIENTED_EDGE('',*,*,#5777,.T.);
#7523=ORIENTED_EDGE('',*,*,#5778,.F.);
#7524=ORIENTED_EDGE('',*,*,#5777,.F.);
#7525=ORIENTED_EDGE('',*,*,#5779,.T.);
#7526=ORIENTED_EDGE('',*,*,#5780,.F.);
#7527=ORIENTED_EDGE('',*,*,#5781,.F.);
#7528=ORIENTED_EDGE('',*,*,#5782,.T.);
#7529=ORIENTED_EDGE('',*,*,#5783,.T.);
#7530=ORIENTED_EDGE('',*,*,#5784,.F.);
#7531=ORIENTED_EDGE('',*,*,#5785,.F.);
#7532=ORIENTED_EDGE('',*,*,#5780,.T.);
#7533=ORIENTED_EDGE('',*,*,#5786,.T.);
#7534=ORIENTED_EDGE('',*,*,#5787,.F.);
#7535=ORIENTED_EDGE('',*,*,#5788,.F.);
#7536=ORIENTED_EDGE('',*,*,#5784,.T.);
#7537=ORIENTED_EDGE('',*,*,#5789,.T.);
#7538=ORIENTED_EDGE('',*,*,#5782,.F.);
#7539=ORIENTED_EDGE('',*,*,#5790,.F.);
#7540=ORIENTED_EDGE('',*,*,#5787,.T.);
#7541=ORIENTED_EDGE('',*,*,#5781,.T.);
#7542=ORIENTED_EDGE('',*,*,#5785,.T.);
#7543=ORIENTED_EDGE('',*,*,#5788,.T.);
#7544=ORIENTED_EDGE('',*,*,#5790,.T.);
#7545=ORIENTED_EDGE('',*,*,#5773,.F.);
#7546=ORIENTED_EDGE('',*,*,#5776,.F.);
#7547=ORIENTED_EDGE('',*,*,#5779,.F.);
#7548=ORIENTED_EDGE('',*,*,#5789,.F.);
#7549=ORIENTED_EDGE('',*,*,#5786,.F.);
#7550=ORIENTED_EDGE('',*,*,#5783,.F.);
#7551=ORIENTED_EDGE('',*,*,#5772,.T.);
#7552=ORIENTED_EDGE('',*,*,#5769,.T.);
#7553=ORIENTED_EDGE('',*,*,#5770,.F.);
#7554=ORIENTED_EDGE('',*,*,#5775,.T.);
#7555=ORIENTED_EDGE('',*,*,#5767,.F.);
#7556=ORIENTED_EDGE('',*,*,#5778,.T.);
#7557=ORIENTED_EDGE('',*,*,#5791,.F.);
#7558=ORIENTED_EDGE('',*,*,#5792,.T.);
#7559=ORIENTED_EDGE('',*,*,#5793,.T.);
#7560=ORIENTED_EDGE('',*,*,#5792,.F.);
#7561=ORIENTED_EDGE('',*,*,#5794,.F.);
#7562=ORIENTED_EDGE('',*,*,#5795,.T.);
#7563=ORIENTED_EDGE('',*,*,#5796,.T.);
#7564=ORIENTED_EDGE('',*,*,#5795,.F.);
#7565=ORIENTED_EDGE('',*,*,#5797,.F.);
#7566=ORIENTED_EDGE('',*,*,#5798,.T.);
#7567=ORIENTED_EDGE('',*,*,#5799,.T.);
#7568=ORIENTED_EDGE('',*,*,#5798,.F.);
#7569=ORIENTED_EDGE('',*,*,#5800,.F.);
#7570=ORIENTED_EDGE('',*,*,#5801,.T.);
#7571=ORIENTED_EDGE('',*,*,#5802,.T.);
#7572=ORIENTED_EDGE('',*,*,#5801,.F.);
#7573=ORIENTED_EDGE('',*,*,#5803,.F.);
#7574=ORIENTED_EDGE('',*,*,#5804,.T.);
#7575=ORIENTED_EDGE('',*,*,#5805,.T.);
#7576=ORIENTED_EDGE('',*,*,#5804,.F.);
#7577=ORIENTED_EDGE('',*,*,#5803,.T.);
#7578=ORIENTED_EDGE('',*,*,#5800,.T.);
#7579=ORIENTED_EDGE('',*,*,#5805,.F.);
#7580=ORIENTED_EDGE('',*,*,#5797,.T.);
#7581=ORIENTED_EDGE('',*,*,#5802,.F.);
#7582=ORIENTED_EDGE('',*,*,#5799,.F.);
#7583=ORIENTED_EDGE('',*,*,#5794,.T.);
#7584=ORIENTED_EDGE('',*,*,#5796,.F.);
#7585=ORIENTED_EDGE('',*,*,#5791,.T.);
#7586=ORIENTED_EDGE('',*,*,#5793,.F.);
#7587=ORIENTED_EDGE('',*,*,#5806,.F.);
#7588=ORIENTED_EDGE('',*,*,#5807,.T.);
#7589=ORIENTED_EDGE('',*,*,#5808,.T.);
#7590=ORIENTED_EDGE('',*,*,#5807,.F.);
#7591=ORIENTED_EDGE('',*,*,#5809,.F.);
#7592=ORIENTED_EDGE('',*,*,#5810,.T.);
#7593=ORIENTED_EDGE('',*,*,#5811,.T.);
#7594=ORIENTED_EDGE('',*,*,#5810,.F.);
#7595=ORIENTED_EDGE('',*,*,#5812,.F.);
#7596=ORIENTED_EDGE('',*,*,#5813,.T.);
#7597=ORIENTED_EDGE('',*,*,#5814,.T.);
#7598=ORIENTED_EDGE('',*,*,#5813,.F.);
#7599=ORIENTED_EDGE('',*,*,#5815,.F.);
#7600=ORIENTED_EDGE('',*,*,#5816,.T.);
#7601=ORIENTED_EDGE('',*,*,#5817,.T.);
#7602=ORIENTED_EDGE('',*,*,#5816,.F.);
#7603=ORIENTED_EDGE('',*,*,#5818,.F.);
#7604=ORIENTED_EDGE('',*,*,#5819,.T.);
#7605=ORIENTED_EDGE('',*,*,#5820,.T.);
#7606=ORIENTED_EDGE('',*,*,#5819,.F.);
#7607=ORIENTED_EDGE('',*,*,#5818,.T.);
#7608=ORIENTED_EDGE('',*,*,#5815,.T.);
#7609=ORIENTED_EDGE('',*,*,#5820,.F.);
#7610=ORIENTED_EDGE('',*,*,#5812,.T.);
#7611=ORIENTED_EDGE('',*,*,#5817,.F.);
#7612=ORIENTED_EDGE('',*,*,#5814,.F.);
#7613=ORIENTED_EDGE('',*,*,#5809,.T.);
#7614=ORIENTED_EDGE('',*,*,#5806,.T.);
#7615=ORIENTED_EDGE('',*,*,#5811,.F.);
#7616=ORIENTED_EDGE('',*,*,#5808,.F.);
#7617=ORIENTED_EDGE('',*,*,#5821,.F.);
#7618=ORIENTED_EDGE('',*,*,#5822,.T.);
#7619=ORIENTED_EDGE('',*,*,#5823,.T.);
#7620=ORIENTED_EDGE('',*,*,#5824,.T.);
#7621=ORIENTED_EDGE('',*,*,#5822,.F.);
#7622=ORIENTED_EDGE('',*,*,#5825,.T.);
#7623=ORIENTED_EDGE('',*,*,#5826,.T.);
#7624=ORIENTED_EDGE('',*,*,#5827,.F.);
#7625=ORIENTED_EDGE('',*,*,#5826,.F.);
#7626=ORIENTED_EDGE('',*,*,#5828,.T.);
#7627=ORIENTED_EDGE('',*,*,#5829,.F.);
#7628=ORIENTED_EDGE('',*,*,#5830,.T.);
#7629=ORIENTED_EDGE('',*,*,#5831,.T.);
#7630=ORIENTED_EDGE('',*,*,#5830,.F.);
#7631=ORIENTED_EDGE('',*,*,#5832,.F.);
#7632=ORIENTED_EDGE('',*,*,#5833,.T.);
#7633=ORIENTED_EDGE('',*,*,#5834,.T.);
#7634=ORIENTED_EDGE('',*,*,#5833,.F.);
#7635=ORIENTED_EDGE('',*,*,#5835,.F.);
#7636=ORIENTED_EDGE('',*,*,#5836,.F.);
#7637=ORIENTED_EDGE('',*,*,#5837,.T.);
#7638=ORIENTED_EDGE('',*,*,#5838,.F.);
#7639=ORIENTED_EDGE('',*,*,#5839,.F.);
#7640=ORIENTED_EDGE('',*,*,#5840,.T.);
#7641=ORIENTED_EDGE('',*,*,#5825,.F.);
#7642=ORIENTED_EDGE('',*,*,#5841,.T.);
#7643=ORIENTED_EDGE('',*,*,#5842,.T.);
#7644=ORIENTED_EDGE('',*,*,#5841,.F.);
#7645=ORIENTED_EDGE('',*,*,#5828,.F.);
#7646=ORIENTED_EDGE('',*,*,#5840,.F.);
#7647=ORIENTED_EDGE('',*,*,#5843,.F.);
#7648=ORIENTED_EDGE('',*,*,#5844,.F.);
#7649=ORIENTED_EDGE('',*,*,#5845,.T.);
#7650=ORIENTED_EDGE('',*,*,#5846,.F.);
#7651=ORIENTED_EDGE('',*,*,#5824,.F.);
#7652=ORIENTED_EDGE('',*,*,#5823,.F.);
#7653=ORIENTED_EDGE('',*,*,#5847,.F.);
#7654=ORIENTED_EDGE('',*,*,#5835,.T.);
#7655=ORIENTED_EDGE('',*,*,#5848,.F.);
#7656=ORIENTED_EDGE('',*,*,#5843,.T.);
#7657=ORIENTED_EDGE('',*,*,#5839,.T.);
#7658=ORIENTED_EDGE('',*,*,#5842,.F.);
#7659=ORIENTED_EDGE('',*,*,#5832,.T.);
#7660=ORIENTED_EDGE('',*,*,#5834,.F.);
#7661=ORIENTED_EDGE('',*,*,#5829,.T.);
#7662=ORIENTED_EDGE('',*,*,#5831,.F.);
#7663=ORIENTED_EDGE('',*,*,#5836,.T.);
#7664=ORIENTED_EDGE('',*,*,#5847,.T.);
#7665=ORIENTED_EDGE('',*,*,#5846,.T.);
#7666=ORIENTED_EDGE('',*,*,#5849,.T.);
#7667=ORIENTED_EDGE('',*,*,#5821,.T.);
#7668=ORIENTED_EDGE('',*,*,#5844,.T.);
#7669=ORIENTED_EDGE('',*,*,#5848,.T.);
#7670=ORIENTED_EDGE('',*,*,#5838,.T.);
#7671=ORIENTED_EDGE('',*,*,#5850,.T.);
#7672=ORIENTED_EDGE('',*,*,#5827,.T.);
#7673=ORIENTED_EDGE('',*,*,#5850,.F.);
#7674=ORIENTED_EDGE('',*,*,#5837,.F.);
#7675=ORIENTED_EDGE('',*,*,#5849,.F.);
#7676=ORIENTED_EDGE('',*,*,#5845,.F.);
#7677=ORIENTED_EDGE('',*,*,#5851,.T.);
#7678=ORIENTED_EDGE('',*,*,#5852,.T.);
#7679=ORIENTED_EDGE('',*,*,#5853,.F.);
#7680=ORIENTED_EDGE('',*,*,#5852,.F.);
#7681=ORIENTED_EDGE('',*,*,#5854,.T.);
#7682=ORIENTED_EDGE('',*,*,#5855,.T.);
#7683=ORIENTED_EDGE('',*,*,#5856,.T.);
#7684=ORIENTED_EDGE('',*,*,#5857,.T.);
#7685=ORIENTED_EDGE('',*,*,#5851,.F.);
#7686=ORIENTED_EDGE('',*,*,#5858,.F.);
#7687=ORIENTED_EDGE('',*,*,#5859,.F.);
#7688=ORIENTED_EDGE('',*,*,#5860,.F.);
#7689=ORIENTED_EDGE('',*,*,#5861,.F.);
#7690=ORIENTED_EDGE('',*,*,#5853,.T.);
#7691=ORIENTED_EDGE('',*,*,#5858,.T.);
#7692=ORIENTED_EDGE('',*,*,#5862,.F.);
#7693=ORIENTED_EDGE('',*,*,#5854,.F.);
#7694=ORIENTED_EDGE('',*,*,#5863,.T.);
#7695=ORIENTED_EDGE('',*,*,#5861,.T.);
#7696=ORIENTED_EDGE('',*,*,#5864,.F.);
#7697=ORIENTED_EDGE('',*,*,#5855,.F.);
#7698=ORIENTED_EDGE('',*,*,#5862,.T.);
#7699=ORIENTED_EDGE('',*,*,#5860,.T.);
#7700=ORIENTED_EDGE('',*,*,#5865,.F.);
#7701=ORIENTED_EDGE('',*,*,#5856,.F.);
#7702=ORIENTED_EDGE('',*,*,#5864,.T.);
#7703=ORIENTED_EDGE('',*,*,#5859,.T.);
#7704=ORIENTED_EDGE('',*,*,#5863,.F.);
#7705=ORIENTED_EDGE('',*,*,#5857,.F.);
#7706=ORIENTED_EDGE('',*,*,#5865,.T.);
#7707=ORIENTED_EDGE('',*,*,#5866,.T.);
#7708=ORIENTED_EDGE('',*,*,#5867,.T.);
#7709=ORIENTED_EDGE('',*,*,#5868,.F.);
#7710=ORIENTED_EDGE('',*,*,#5867,.F.);
#7711=ORIENTED_EDGE('',*,*,#5869,.T.);
#7712=ORIENTED_EDGE('',*,*,#5870,.T.);
#7713=ORIENTED_EDGE('',*,*,#5871,.T.);
#7714=ORIENTED_EDGE('',*,*,#5872,.T.);
#7715=ORIENTED_EDGE('',*,*,#5866,.F.);
#7716=ORIENTED_EDGE('',*,*,#5873,.F.);
#7717=ORIENTED_EDGE('',*,*,#5874,.F.);
#7718=ORIENTED_EDGE('',*,*,#5875,.F.);
#7719=ORIENTED_EDGE('',*,*,#5876,.F.);
#7720=ORIENTED_EDGE('',*,*,#5868,.T.);
#7721=ORIENTED_EDGE('',*,*,#5873,.T.);
#7722=ORIENTED_EDGE('',*,*,#5877,.F.);
#7723=ORIENTED_EDGE('',*,*,#5869,.F.);
#7724=ORIENTED_EDGE('',*,*,#5878,.T.);
#7725=ORIENTED_EDGE('',*,*,#5876,.T.);
#7726=ORIENTED_EDGE('',*,*,#5879,.F.);
#7727=ORIENTED_EDGE('',*,*,#5870,.F.);
#7728=ORIENTED_EDGE('',*,*,#5877,.T.);
#7729=ORIENTED_EDGE('',*,*,#5875,.T.);
#7730=ORIENTED_EDGE('',*,*,#5880,.F.);
#7731=ORIENTED_EDGE('',*,*,#5871,.F.);
#7732=ORIENTED_EDGE('',*,*,#5879,.T.);
#7733=ORIENTED_EDGE('',*,*,#5874,.T.);
#7734=ORIENTED_EDGE('',*,*,#5878,.F.);
#7735=ORIENTED_EDGE('',*,*,#5872,.F.);
#7736=ORIENTED_EDGE('',*,*,#5880,.T.);
#7737=ORIENTED_EDGE('',*,*,#5881,.F.);
#7738=ORIENTED_EDGE('',*,*,#5882,.T.);
#7739=ORIENTED_EDGE('',*,*,#5883,.T.);
#7740=ORIENTED_EDGE('',*,*,#5882,.F.);
#7741=ORIENTED_EDGE('',*,*,#5884,.F.);
#7742=ORIENTED_EDGE('',*,*,#5885,.T.);
#7743=ORIENTED_EDGE('',*,*,#5886,.T.);
#7744=ORIENTED_EDGE('',*,*,#5887,.T.);
#7745=ORIENTED_EDGE('',*,*,#5888,.T.);
#7746=ORIENTED_EDGE('',*,*,#5889,.T.);
#7747=ORIENTED_EDGE('',*,*,#5890,.F.);
#7748=ORIENTED_EDGE('',*,*,#5889,.F.);
#7749=ORIENTED_EDGE('',*,*,#5891,.T.);
#7750=ORIENTED_EDGE('',*,*,#5892,.T.);
#7751=ORIENTED_EDGE('',*,*,#5887,.F.);
#7752=ORIENTED_EDGE('',*,*,#5885,.F.);
#7753=ORIENTED_EDGE('',*,*,#5892,.F.);
#7754=ORIENTED_EDGE('',*,*,#5890,.T.);
#7755=ORIENTED_EDGE('',*,*,#5891,.F.);
#7756=ORIENTED_EDGE('',*,*,#5888,.F.);
#7757=ORIENTED_EDGE('',*,*,#5884,.T.);
#7758=ORIENTED_EDGE('',*,*,#5881,.T.);
#7759=ORIENTED_EDGE('',*,*,#5886,.F.);
#7760=ORIENTED_EDGE('',*,*,#5883,.F.);
#7761=ORIENTED_EDGE('',*,*,#5893,.T.);
#7762=ORIENTED_EDGE('',*,*,#5894,.T.);
#7763=ORIENTED_EDGE('',*,*,#5895,.F.);
#7764=ORIENTED_EDGE('',*,*,#5894,.F.);
#7765=ORIENTED_EDGE('',*,*,#5895,.T.);
#7766=ORIENTED_EDGE('',*,*,#5893,.F.);
#7767=ORIENTED_EDGE('',*,*,#5896,.T.);
#7768=ORIENTED_EDGE('',*,*,#5897,.T.);
#7769=ORIENTED_EDGE('',*,*,#5898,.F.);
#7770=ORIENTED_EDGE('',*,*,#5897,.F.);
#7771=ORIENTED_EDGE('',*,*,#5899,.T.);
#7772=ORIENTED_EDGE('',*,*,#5900,.T.);
#7773=ORIENTED_EDGE('',*,*,#5901,.F.);
#7774=ORIENTED_EDGE('',*,*,#5900,.F.);
#7775=ORIENTED_EDGE('',*,*,#5902,.F.);
#7776=ORIENTED_EDGE('',*,*,#5903,.T.);
#7777=ORIENTED_EDGE('',*,*,#5904,.F.);
#7778=ORIENTED_EDGE('',*,*,#5903,.F.);
#7779=ORIENTED_EDGE('',*,*,#5905,.F.);
#7780=ORIENTED_EDGE('',*,*,#5906,.T.);
#7781=ORIENTED_EDGE('',*,*,#5907,.F.);
#7782=ORIENTED_EDGE('',*,*,#5906,.F.);
#7783=ORIENTED_EDGE('',*,*,#5908,.T.);
#7784=ORIENTED_EDGE('',*,*,#5909,.F.);
#7785=ORIENTED_EDGE('',*,*,#5910,.F.);
#7786=ORIENTED_EDGE('',*,*,#5911,.T.);
#7787=ORIENTED_EDGE('',*,*,#5912,.T.);
#7788=ORIENTED_EDGE('',*,*,#5913,.F.);
#7789=ORIENTED_EDGE('',*,*,#5914,.F.);
#7790=ORIENTED_EDGE('',*,*,#5909,.T.);
#7791=ORIENTED_EDGE('',*,*,#5915,.T.);
#7792=ORIENTED_EDGE('',*,*,#5916,.F.);
#7793=ORIENTED_EDGE('',*,*,#5917,.F.);
#7794=ORIENTED_EDGE('',*,*,#5913,.T.);
#7795=ORIENTED_EDGE('',*,*,#5918,.T.);
#7796=ORIENTED_EDGE('',*,*,#5911,.F.);
#7797=ORIENTED_EDGE('',*,*,#5919,.F.);
#7798=ORIENTED_EDGE('',*,*,#5916,.T.);
#7799=ORIENTED_EDGE('',*,*,#5910,.T.);
#7800=ORIENTED_EDGE('',*,*,#5914,.T.);
#7801=ORIENTED_EDGE('',*,*,#5917,.T.);
#7802=ORIENTED_EDGE('',*,*,#5919,.T.);
#7803=ORIENTED_EDGE('',*,*,#5902,.T.);
#7804=ORIENTED_EDGE('',*,*,#5905,.T.);
#7805=ORIENTED_EDGE('',*,*,#5908,.F.);
#7806=ORIENTED_EDGE('',*,*,#5918,.F.);
#7807=ORIENTED_EDGE('',*,*,#5915,.F.);
#7808=ORIENTED_EDGE('',*,*,#5912,.F.);
#7809=ORIENTED_EDGE('',*,*,#5901,.T.);
#7810=ORIENTED_EDGE('',*,*,#5898,.T.);
#7811=ORIENTED_EDGE('',*,*,#5899,.F.);
#7812=ORIENTED_EDGE('',*,*,#5904,.T.);
#7813=ORIENTED_EDGE('',*,*,#5896,.F.);
#7814=ORIENTED_EDGE('',*,*,#5907,.T.);
#7815=ORIENTED_EDGE('',*,*,#5920,.T.);
#7816=ORIENTED_EDGE('',*,*,#5921,.T.);
#7817=ORIENTED_EDGE('',*,*,#5922,.F.);
#7818=ORIENTED_EDGE('',*,*,#5921,.F.);
#7819=ORIENTED_EDGE('',*,*,#5923,.T.);
#7820=ORIENTED_EDGE('',*,*,#5924,.T.);
#7821=ORIENTED_EDGE('',*,*,#5925,.F.);
#7822=ORIENTED_EDGE('',*,*,#5924,.F.);
#7823=ORIENTED_EDGE('',*,*,#5926,.T.);
#7824=ORIENTED_EDGE('',*,*,#5927,.T.);
#7825=ORIENTED_EDGE('',*,*,#5928,.F.);
#7826=ORIENTED_EDGE('',*,*,#5927,.F.);
#7827=ORIENTED_EDGE('',*,*,#5929,.T.);
#7828=ORIENTED_EDGE('',*,*,#5930,.T.);
#7829=ORIENTED_EDGE('',*,*,#5931,.T.);
#7830=ORIENTED_EDGE('',*,*,#5932,.T.);
#7831=ORIENTED_EDGE('',*,*,#5933,.T.);
#7832=ORIENTED_EDGE('',*,*,#5934,.T.);
#7833=ORIENTED_EDGE('',*,*,#5935,.T.);
#7834=ORIENTED_EDGE('',*,*,#5936,.T.);
#7835=ORIENTED_EDGE('',*,*,#5926,.F.);
#7836=ORIENTED_EDGE('',*,*,#5920,.F.);
#7837=ORIENTED_EDGE('',*,*,#5923,.F.);
#7838=ORIENTED_EDGE('',*,*,#5937,.F.);
#7839=ORIENTED_EDGE('',*,*,#5938,.F.);
#7840=ORIENTED_EDGE('',*,*,#5939,.F.);
#7841=ORIENTED_EDGE('',*,*,#5940,.F.);
#7842=ORIENTED_EDGE('',*,*,#5941,.F.);
#7843=ORIENTED_EDGE('',*,*,#5942,.F.);
#7844=ORIENTED_EDGE('',*,*,#5943,.F.);
#7845=ORIENTED_EDGE('',*,*,#5944,.F.);
#7846=ORIENTED_EDGE('',*,*,#5928,.T.);
#7847=ORIENTED_EDGE('',*,*,#5925,.T.);
#7848=ORIENTED_EDGE('',*,*,#5922,.T.);
#7849=ORIENTED_EDGE('',*,*,#5937,.T.);
#7850=ORIENTED_EDGE('',*,*,#5945,.F.);
#7851=ORIENTED_EDGE('',*,*,#5929,.F.);
#7852=ORIENTED_EDGE('',*,*,#5946,.T.);
#7853=ORIENTED_EDGE('',*,*,#5944,.T.);
#7854=ORIENTED_EDGE('',*,*,#5947,.F.);
#7855=ORIENTED_EDGE('',*,*,#5930,.F.);
#7856=ORIENTED_EDGE('',*,*,#5945,.T.);
#7857=ORIENTED_EDGE('',*,*,#5943,.T.);
#7858=ORIENTED_EDGE('',*,*,#5948,.F.);
#7859=ORIENTED_EDGE('',*,*,#5931,.F.);
#7860=ORIENTED_EDGE('',*,*,#5947,.T.);
#7861=ORIENTED_EDGE('',*,*,#5942,.T.);
#7862=ORIENTED_EDGE('',*,*,#5949,.F.);
#7863=ORIENTED_EDGE('',*,*,#5932,.F.);
#7864=ORIENTED_EDGE('',*,*,#5948,.T.);
#7865=ORIENTED_EDGE('',*,*,#5941,.T.);
#7866=ORIENTED_EDGE('',*,*,#5950,.F.);
#7867=ORIENTED_EDGE('',*,*,#5933,.F.);
#7868=ORIENTED_EDGE('',*,*,#5949,.T.);
#7869=ORIENTED_EDGE('',*,*,#5940,.T.);
#7870=ORIENTED_EDGE('',*,*,#5951,.F.);
#7871=ORIENTED_EDGE('',*,*,#5934,.F.);
#7872=ORIENTED_EDGE('',*,*,#5950,.T.);
#7873=ORIENTED_EDGE('',*,*,#5939,.T.);
#7874=ORIENTED_EDGE('',*,*,#5952,.F.);
#7875=ORIENTED_EDGE('',*,*,#5935,.F.);
#7876=ORIENTED_EDGE('',*,*,#5951,.T.);
#7877=ORIENTED_EDGE('',*,*,#5938,.T.);
#7878=ORIENTED_EDGE('',*,*,#5946,.F.);
#7879=ORIENTED_EDGE('',*,*,#5936,.F.);
#7880=ORIENTED_EDGE('',*,*,#5952,.T.);
#7881=ORIENTED_EDGE('',*,*,#5953,.T.);
#7882=ORIENTED_EDGE('',*,*,#5954,.T.);
#7883=ORIENTED_EDGE('',*,*,#5955,.F.);
#7884=ORIENTED_EDGE('',*,*,#5954,.F.);
#7885=ORIENTED_EDGE('',*,*,#5956,.T.);
#7886=ORIENTED_EDGE('',*,*,#5957,.T.);
#7887=ORIENTED_EDGE('',*,*,#5958,.F.);
#7888=ORIENTED_EDGE('',*,*,#5959,.F.);
#7889=ORIENTED_EDGE('',*,*,#5960,.T.);
#7890=ORIENTED_EDGE('',*,*,#5961,.T.);
#7891=ORIENTED_EDGE('',*,*,#5962,.F.);
#7892=ORIENTED_EDGE('',*,*,#5961,.F.);
#7893=ORIENTED_EDGE('',*,*,#5963,.T.);
#7894=ORIENTED_EDGE('',*,*,#5964,.F.);
#7895=ORIENTED_EDGE('',*,*,#5965,.F.);
#7896=ORIENTED_EDGE('',*,*,#5957,.F.);
#7897=ORIENTED_EDGE('',*,*,#5966,.T.);
#7898=ORIENTED_EDGE('',*,*,#5967,.F.);
#7899=ORIENTED_EDGE('',*,*,#5968,.F.);
#7900=ORIENTED_EDGE('',*,*,#5969,.F.);
#7901=ORIENTED_EDGE('',*,*,#5970,.F.);
#7902=ORIENTED_EDGE('',*,*,#5971,.T.);
#7903=ORIENTED_EDGE('',*,*,#5972,.F.);
#7904=ORIENTED_EDGE('',*,*,#5973,.F.);
#7905=ORIENTED_EDGE('',*,*,#5974,.F.);
#7906=ORIENTED_EDGE('',*,*,#5975,.T.);
#7907=ORIENTED_EDGE('',*,*,#5976,.F.);
#7908=ORIENTED_EDGE('',*,*,#5977,.F.);
#7909=ORIENTED_EDGE('',*,*,#5978,.F.);
#7910=ORIENTED_EDGE('',*,*,#5979,.T.);
#7911=ORIENTED_EDGE('',*,*,#5980,.F.);
#7912=ORIENTED_EDGE('',*,*,#5981,.F.);
#7913=ORIENTED_EDGE('',*,*,#5982,.F.);
#7914=ORIENTED_EDGE('',*,*,#5983,.T.);
#7915=ORIENTED_EDGE('',*,*,#5984,.F.);
#7916=ORIENTED_EDGE('',*,*,#5985,.F.);
#7917=ORIENTED_EDGE('',*,*,#5986,.F.);
#7918=ORIENTED_EDGE('',*,*,#5987,.T.);
#7919=ORIENTED_EDGE('',*,*,#5988,.F.);
#7920=ORIENTED_EDGE('',*,*,#5989,.F.);
#7921=ORIENTED_EDGE('',*,*,#5990,.F.);
#7922=ORIENTED_EDGE('',*,*,#5991,.T.);
#7923=ORIENTED_EDGE('',*,*,#5992,.F.);
#7924=ORIENTED_EDGE('',*,*,#5993,.F.);
#7925=ORIENTED_EDGE('',*,*,#5994,.F.);
#7926=ORIENTED_EDGE('',*,*,#5995,.T.);
#7927=ORIENTED_EDGE('',*,*,#5996,.F.);
#7928=ORIENTED_EDGE('',*,*,#5997,.F.);
#7929=ORIENTED_EDGE('',*,*,#5998,.F.);
#7930=ORIENTED_EDGE('',*,*,#5999,.T.);
#7931=ORIENTED_EDGE('',*,*,#6000,.F.);
#7932=ORIENTED_EDGE('',*,*,#6001,.F.);
#7933=ORIENTED_EDGE('',*,*,#6002,.F.);
#7934=ORIENTED_EDGE('',*,*,#6003,.T.);
#7935=ORIENTED_EDGE('',*,*,#6004,.F.);
#7936=ORIENTED_EDGE('',*,*,#6005,.F.);
#7937=ORIENTED_EDGE('',*,*,#6006,.F.);
#7938=ORIENTED_EDGE('',*,*,#6007,.T.);
#7939=ORIENTED_EDGE('',*,*,#6008,.F.);
#7940=ORIENTED_EDGE('',*,*,#6009,.F.);
#7941=ORIENTED_EDGE('',*,*,#6010,.F.);
#7942=ORIENTED_EDGE('',*,*,#6011,.T.);
#7943=ORIENTED_EDGE('',*,*,#6012,.F.);
#7944=ORIENTED_EDGE('',*,*,#6013,.F.);
#7945=ORIENTED_EDGE('',*,*,#6014,.F.);
#7946=ORIENTED_EDGE('',*,*,#6015,.T.);
#7947=ORIENTED_EDGE('',*,*,#6016,.F.);
#7948=ORIENTED_EDGE('',*,*,#6017,.F.);
#7949=ORIENTED_EDGE('',*,*,#6018,.F.);
#7950=ORIENTED_EDGE('',*,*,#6019,.T.);
#7951=ORIENTED_EDGE('',*,*,#6020,.F.);
#7952=ORIENTED_EDGE('',*,*,#6021,.F.);
#7953=ORIENTED_EDGE('',*,*,#6022,.F.);
#7954=ORIENTED_EDGE('',*,*,#6023,.T.);
#7955=ORIENTED_EDGE('',*,*,#6024,.F.);
#7956=ORIENTED_EDGE('',*,*,#6025,.F.);
#7957=ORIENTED_EDGE('',*,*,#6026,.F.);
#7958=ORIENTED_EDGE('',*,*,#6027,.T.);
#7959=ORIENTED_EDGE('',*,*,#6028,.F.);
#7960=ORIENTED_EDGE('',*,*,#6029,.F.);
#7961=ORIENTED_EDGE('',*,*,#6030,.F.);
#7962=ORIENTED_EDGE('',*,*,#6031,.T.);
#7963=ORIENTED_EDGE('',*,*,#6032,.F.);
#7964=ORIENTED_EDGE('',*,*,#6033,.F.);
#7965=ORIENTED_EDGE('',*,*,#6034,.F.);
#7966=ORIENTED_EDGE('',*,*,#6035,.T.);
#7967=ORIENTED_EDGE('',*,*,#6036,.F.);
#7968=ORIENTED_EDGE('',*,*,#6037,.F.);
#7969=ORIENTED_EDGE('',*,*,#6038,.F.);
#7970=ORIENTED_EDGE('',*,*,#6039,.T.);
#7971=ORIENTED_EDGE('',*,*,#6040,.F.);
#7972=ORIENTED_EDGE('',*,*,#6041,.F.);
#7973=ORIENTED_EDGE('',*,*,#6042,.F.);
#7974=ORIENTED_EDGE('',*,*,#6043,.T.);
#7975=ORIENTED_EDGE('',*,*,#6044,.F.);
#7976=ORIENTED_EDGE('',*,*,#6045,.F.);
#7977=ORIENTED_EDGE('',*,*,#6046,.F.);
#7978=ORIENTED_EDGE('',*,*,#6047,.T.);
#7979=ORIENTED_EDGE('',*,*,#6048,.F.);
#7980=ORIENTED_EDGE('',*,*,#6049,.F.);
#7981=ORIENTED_EDGE('',*,*,#6050,.F.);
#7982=ORIENTED_EDGE('',*,*,#6051,.T.);
#7983=ORIENTED_EDGE('',*,*,#6052,.F.);
#7984=ORIENTED_EDGE('',*,*,#6053,.F.);
#7985=ORIENTED_EDGE('',*,*,#6054,.F.);
#7986=ORIENTED_EDGE('',*,*,#6055,.T.);
#7987=ORIENTED_EDGE('',*,*,#6056,.F.);
#7988=ORIENTED_EDGE('',*,*,#6057,.F.);
#7989=ORIENTED_EDGE('',*,*,#6058,.F.);
#7990=ORIENTED_EDGE('',*,*,#6059,.T.);
#7991=ORIENTED_EDGE('',*,*,#6060,.F.);
#7992=ORIENTED_EDGE('',*,*,#6061,.F.);
#7993=ORIENTED_EDGE('',*,*,#6062,.F.);
#7994=ORIENTED_EDGE('',*,*,#6063,.T.);
#7995=ORIENTED_EDGE('',*,*,#6064,.F.);
#7996=ORIENTED_EDGE('',*,*,#6065,.F.);
#7997=ORIENTED_EDGE('',*,*,#6066,.F.);
#7998=ORIENTED_EDGE('',*,*,#6067,.T.);
#7999=ORIENTED_EDGE('',*,*,#6068,.F.);
#8000=ORIENTED_EDGE('',*,*,#6069,.F.);
#8001=ORIENTED_EDGE('',*,*,#6070,.F.);
#8002=ORIENTED_EDGE('',*,*,#6071,.T.);
#8003=ORIENTED_EDGE('',*,*,#6072,.F.);
#8004=ORIENTED_EDGE('',*,*,#6073,.F.);
#8005=ORIENTED_EDGE('',*,*,#6074,.F.);
#8006=ORIENTED_EDGE('',*,*,#6075,.T.);
#8007=ORIENTED_EDGE('',*,*,#6076,.F.);
#8008=ORIENTED_EDGE('',*,*,#6077,.F.);
#8009=ORIENTED_EDGE('',*,*,#6078,.F.);
#8010=ORIENTED_EDGE('',*,*,#6079,.T.);
#8011=ORIENTED_EDGE('',*,*,#6080,.F.);
#8012=ORIENTED_EDGE('',*,*,#6081,.F.);
#8013=ORIENTED_EDGE('',*,*,#6082,.F.);
#8014=ORIENTED_EDGE('',*,*,#6083,.T.);
#8015=ORIENTED_EDGE('',*,*,#6084,.F.);
#8016=ORIENTED_EDGE('',*,*,#6085,.F.);
#8017=ORIENTED_EDGE('',*,*,#6086,.F.);
#8018=ORIENTED_EDGE('',*,*,#6087,.T.);
#8019=ORIENTED_EDGE('',*,*,#6088,.F.);
#8020=ORIENTED_EDGE('',*,*,#6089,.F.);
#8021=ORIENTED_EDGE('',*,*,#6090,.F.);
#8022=ORIENTED_EDGE('',*,*,#6091,.T.);
#8023=ORIENTED_EDGE('',*,*,#6092,.F.);
#8024=ORIENTED_EDGE('',*,*,#6093,.F.);
#8025=ORIENTED_EDGE('',*,*,#6094,.F.);
#8026=ORIENTED_EDGE('',*,*,#6095,.T.);
#8027=ORIENTED_EDGE('',*,*,#6096,.F.);
#8028=ORIENTED_EDGE('',*,*,#6097,.F.);
#8029=ORIENTED_EDGE('',*,*,#6098,.F.);
#8030=ORIENTED_EDGE('',*,*,#6099,.T.);
#8031=ORIENTED_EDGE('',*,*,#6100,.F.);
#8032=ORIENTED_EDGE('',*,*,#6101,.F.);
#8033=ORIENTED_EDGE('',*,*,#6102,.F.);
#8034=ORIENTED_EDGE('',*,*,#6103,.T.);
#8035=ORIENTED_EDGE('',*,*,#6104,.F.);
#8036=ORIENTED_EDGE('',*,*,#6105,.F.);
#8037=ORIENTED_EDGE('',*,*,#6106,.F.);
#8038=ORIENTED_EDGE('',*,*,#6107,.T.);
#8039=ORIENTED_EDGE('',*,*,#6108,.F.);
#8040=ORIENTED_EDGE('',*,*,#6109,.F.);
#8041=ORIENTED_EDGE('',*,*,#6110,.F.);
#8042=ORIENTED_EDGE('',*,*,#6111,.T.);
#8043=ORIENTED_EDGE('',*,*,#6112,.F.);
#8044=ORIENTED_EDGE('',*,*,#6113,.F.);
#8045=ORIENTED_EDGE('',*,*,#6114,.F.);
#8046=ORIENTED_EDGE('',*,*,#6115,.T.);
#8047=ORIENTED_EDGE('',*,*,#6116,.F.);
#8048=ORIENTED_EDGE('',*,*,#6117,.F.);
#8049=ORIENTED_EDGE('',*,*,#6118,.F.);
#8050=ORIENTED_EDGE('',*,*,#6119,.T.);
#8051=ORIENTED_EDGE('',*,*,#6120,.F.);
#8052=ORIENTED_EDGE('',*,*,#6121,.F.);
#8053=ORIENTED_EDGE('',*,*,#5962,.T.);
#8054=ORIENTED_EDGE('',*,*,#5953,.F.);
#8055=ORIENTED_EDGE('',*,*,#5956,.F.);
#8056=ORIENTED_EDGE('',*,*,#5955,.T.);
#8057=ORIENTED_EDGE('',*,*,#5970,.T.);
#8058=ORIENTED_EDGE('',*,*,#6122,.F.);
#8059=ORIENTED_EDGE('',*,*,#6123,.F.);
#8060=ORIENTED_EDGE('',*,*,#6124,.T.);
#8061=ORIENTED_EDGE('',*,*,#5972,.T.);
#8062=ORIENTED_EDGE('',*,*,#6125,.T.);
#8063=ORIENTED_EDGE('',*,*,#6126,.T.);
#8064=ORIENTED_EDGE('',*,*,#6127,.F.);
#8065=ORIENTED_EDGE('',*,*,#6124,.F.);
#8066=ORIENTED_EDGE('',*,*,#6128,.F.);
#8067=ORIENTED_EDGE('',*,*,#6125,.F.);
#8068=ORIENTED_EDGE('',*,*,#5971,.F.);
#8069=ORIENTED_EDGE('',*,*,#5973,.T.);
#8070=ORIENTED_EDGE('',*,*,#6127,.T.);
#8071=ORIENTED_EDGE('',*,*,#6129,.T.);
#8072=ORIENTED_EDGE('',*,*,#6122,.T.);
#8073=ORIENTED_EDGE('',*,*,#6129,.F.);
#8074=ORIENTED_EDGE('',*,*,#6126,.F.);
#8075=ORIENTED_EDGE('',*,*,#6128,.T.);
#8076=ORIENTED_EDGE('',*,*,#6123,.T.);
#8077=ORIENTED_EDGE('',*,*,#5974,.T.);
#8078=ORIENTED_EDGE('',*,*,#6130,.F.);
#8079=ORIENTED_EDGE('',*,*,#6131,.F.);
#8080=ORIENTED_EDGE('',*,*,#6132,.T.);
#8081=ORIENTED_EDGE('',*,*,#5976,.T.);
#8082=ORIENTED_EDGE('',*,*,#6133,.T.);
#8083=ORIENTED_EDGE('',*,*,#6134,.T.);
#8084=ORIENTED_EDGE('',*,*,#6135,.F.);
#8085=ORIENTED_EDGE('',*,*,#6132,.F.);
#8086=ORIENTED_EDGE('',*,*,#6136,.F.);
#8087=ORIENTED_EDGE('',*,*,#6133,.F.);
#8088=ORIENTED_EDGE('',*,*,#5975,.F.);
#8089=ORIENTED_EDGE('',*,*,#5977,.T.);
#8090=ORIENTED_EDGE('',*,*,#6135,.T.);
#8091=ORIENTED_EDGE('',*,*,#6137,.T.);
#8092=ORIENTED_EDGE('',*,*,#6130,.T.);
#8093=ORIENTED_EDGE('',*,*,#6137,.F.);
#8094=ORIENTED_EDGE('',*,*,#6134,.F.);
#8095=ORIENTED_EDGE('',*,*,#6136,.T.);
#8096=ORIENTED_EDGE('',*,*,#6131,.T.);
#8097=ORIENTED_EDGE('',*,*,#5978,.T.);
#8098=ORIENTED_EDGE('',*,*,#6138,.F.);
#8099=ORIENTED_EDGE('',*,*,#6139,.F.);
#8100=ORIENTED_EDGE('',*,*,#6140,.T.);
#8101=ORIENTED_EDGE('',*,*,#5980,.T.);
#8102=ORIENTED_EDGE('',*,*,#6141,.T.);
#8103=ORIENTED_EDGE('',*,*,#6142,.T.);
#8104=ORIENTED_EDGE('',*,*,#6143,.F.);
#8105=ORIENTED_EDGE('',*,*,#6140,.F.);
#8106=ORIENTED_EDGE('',*,*,#6144,.F.);
#8107=ORIENTED_EDGE('',*,*,#6141,.F.);
#8108=ORIENTED_EDGE('',*,*,#5979,.F.);
#8109=ORIENTED_EDGE('',*,*,#5981,.T.);
#8110=ORIENTED_EDGE('',*,*,#6143,.T.);
#8111=ORIENTED_EDGE('',*,*,#6145,.T.);
#8112=ORIENTED_EDGE('',*,*,#6138,.T.);
#8113=ORIENTED_EDGE('',*,*,#6145,.F.);
#8114=ORIENTED_EDGE('',*,*,#6142,.F.);
#8115=ORIENTED_EDGE('',*,*,#6144,.T.);
#8116=ORIENTED_EDGE('',*,*,#6139,.T.);
#8117=ORIENTED_EDGE('',*,*,#5969,.T.);
#8118=ORIENTED_EDGE('',*,*,#6146,.F.);
#8119=ORIENTED_EDGE('',*,*,#6147,.F.);
#8120=ORIENTED_EDGE('',*,*,#6148,.T.);
#8121=ORIENTED_EDGE('',*,*,#5967,.T.);
#8122=ORIENTED_EDGE('',*,*,#6149,.T.);
#8123=ORIENTED_EDGE('',*,*,#6150,.T.);
#8124=ORIENTED_EDGE('',*,*,#6151,.F.);
#8125=ORIENTED_EDGE('',*,*,#6148,.F.);
#8126=ORIENTED_EDGE('',*,*,#6152,.F.);
#8127=ORIENTED_EDGE('',*,*,#6149,.F.);
#8128=ORIENTED_EDGE('',*,*,#5966,.F.);
#8129=ORIENTED_EDGE('',*,*,#5968,.T.);
#8130=ORIENTED_EDGE('',*,*,#6151,.T.);
#8131=ORIENTED_EDGE('',*,*,#6153,.T.);
#8132=ORIENTED_EDGE('',*,*,#6146,.T.);
#8133=ORIENTED_EDGE('',*,*,#6153,.F.);
#8134=ORIENTED_EDGE('',*,*,#6150,.F.);
#8135=ORIENTED_EDGE('',*,*,#6152,.T.);
#8136=ORIENTED_EDGE('',*,*,#6147,.T.);
#8137=ORIENTED_EDGE('',*,*,#6046,.T.);
#8138=ORIENTED_EDGE('',*,*,#6154,.F.);
#8139=ORIENTED_EDGE('',*,*,#6155,.F.);
#8140=ORIENTED_EDGE('',*,*,#6156,.T.);
#8141=ORIENTED_EDGE('',*,*,#6048,.T.);
#8142=ORIENTED_EDGE('',*,*,#6157,.T.);
#8143=ORIENTED_EDGE('',*,*,#6158,.T.);
#8144=ORIENTED_EDGE('',*,*,#6159,.F.);
#8145=ORIENTED_EDGE('',*,*,#6156,.F.);
#8146=ORIENTED_EDGE('',*,*,#6160,.F.);
#8147=ORIENTED_EDGE('',*,*,#6157,.F.);
#8148=ORIENTED_EDGE('',*,*,#6047,.F.);
#8149=ORIENTED_EDGE('',*,*,#6049,.T.);
#8150=ORIENTED_EDGE('',*,*,#6159,.T.);
#8151=ORIENTED_EDGE('',*,*,#6161,.T.);
#8152=ORIENTED_EDGE('',*,*,#6154,.T.);
#8153=ORIENTED_EDGE('',*,*,#6161,.F.);
#8154=ORIENTED_EDGE('',*,*,#6158,.F.);
#8155=ORIENTED_EDGE('',*,*,#6160,.T.);
#8156=ORIENTED_EDGE('',*,*,#6155,.T.);
#8157=ORIENTED_EDGE('',*,*,#6050,.T.);
#8158=ORIENTED_EDGE('',*,*,#6162,.F.);
#8159=ORIENTED_EDGE('',*,*,#6163,.F.);
#8160=ORIENTED_EDGE('',*,*,#6164,.T.);
#8161=ORIENTED_EDGE('',*,*,#6052,.T.);
#8162=ORIENTED_EDGE('',*,*,#6165,.T.);
#8163=ORIENTED_EDGE('',*,*,#6166,.T.);
#8164=ORIENTED_EDGE('',*,*,#6167,.F.);
#8165=ORIENTED_EDGE('',*,*,#6164,.F.);
#8166=ORIENTED_EDGE('',*,*,#6168,.F.);
#8167=ORIENTED_EDGE('',*,*,#6165,.F.);
#8168=ORIENTED_EDGE('',*,*,#6051,.F.);
#8169=ORIENTED_EDGE('',*,*,#6053,.T.);
#8170=ORIENTED_EDGE('',*,*,#6167,.T.);
#8171=ORIENTED_EDGE('',*,*,#6169,.T.);
#8172=ORIENTED_EDGE('',*,*,#6162,.T.);
#8173=ORIENTED_EDGE('',*,*,#6169,.F.);
#8174=ORIENTED_EDGE('',*,*,#6166,.F.);
#8175=ORIENTED_EDGE('',*,*,#6168,.T.);
#8176=ORIENTED_EDGE('',*,*,#6163,.T.);
#8177=ORIENTED_EDGE('',*,*,#6054,.T.);
#8178=ORIENTED_EDGE('',*,*,#6170,.F.);
#8179=ORIENTED_EDGE('',*,*,#6171,.F.);
#8180=ORIENTED_EDGE('',*,*,#6172,.T.);
#8181=ORIENTED_EDGE('',*,*,#6056,.T.);
#8182=ORIENTED_EDGE('',*,*,#6173,.T.);
#8183=ORIENTED_EDGE('',*,*,#6174,.T.);
#8184=ORIENTED_EDGE('',*,*,#6175,.F.);
#8185=ORIENTED_EDGE('',*,*,#6172,.F.);
#8186=ORIENTED_EDGE('',*,*,#6176,.F.);
#8187=ORIENTED_EDGE('',*,*,#6173,.F.);
#8188=ORIENTED_EDGE('',*,*,#6055,.F.);
#8189=ORIENTED_EDGE('',*,*,#6057,.T.);
#8190=ORIENTED_EDGE('',*,*,#6175,.T.);
#8191=ORIENTED_EDGE('',*,*,#6177,.T.);
#8192=ORIENTED_EDGE('',*,*,#6170,.T.);
#8193=ORIENTED_EDGE('',*,*,#6177,.F.);
#8194=ORIENTED_EDGE('',*,*,#6174,.F.);
#8195=ORIENTED_EDGE('',*,*,#6176,.T.);
#8196=ORIENTED_EDGE('',*,*,#6171,.T.);
#8197=ORIENTED_EDGE('',*,*,#5959,.T.);
#8198=ORIENTED_EDGE('',*,*,#6178,.F.);
#8199=ORIENTED_EDGE('',*,*,#6179,.F.);
#8200=ORIENTED_EDGE('',*,*,#6180,.T.);
#8201=ORIENTED_EDGE('',*,*,#5964,.T.);
#8202=ORIENTED_EDGE('',*,*,#6181,.T.);
#8203=ORIENTED_EDGE('',*,*,#6182,.T.);
#8204=ORIENTED_EDGE('',*,*,#6183,.F.);
#8205=ORIENTED_EDGE('',*,*,#6180,.F.);
#8206=ORIENTED_EDGE('',*,*,#6184,.F.);
#8207=ORIENTED_EDGE('',*,*,#6181,.F.);
#8208=ORIENTED_EDGE('',*,*,#5963,.F.);
#8209=ORIENTED_EDGE('',*,*,#5960,.F.);
#8210=ORIENTED_EDGE('',*,*,#5958,.T.);
#8211=ORIENTED_EDGE('',*,*,#5965,.T.);
#8212=ORIENTED_EDGE('',*,*,#6183,.T.);
#8213=ORIENTED_EDGE('',*,*,#6185,.T.);
#8214=ORIENTED_EDGE('',*,*,#6178,.T.);
#8215=ORIENTED_EDGE('',*,*,#6185,.F.);
#8216=ORIENTED_EDGE('',*,*,#6182,.F.);
#8217=ORIENTED_EDGE('',*,*,#6184,.T.);
#8218=ORIENTED_EDGE('',*,*,#6179,.T.);
#8219=ORIENTED_EDGE('',*,*,#6058,.T.);
#8220=ORIENTED_EDGE('',*,*,#6186,.F.);
#8221=ORIENTED_EDGE('',*,*,#6187,.F.);
#8222=ORIENTED_EDGE('',*,*,#6188,.T.);
#8223=ORIENTED_EDGE('',*,*,#6060,.T.);
#8224=ORIENTED_EDGE('',*,*,#6189,.T.);
#8225=ORIENTED_EDGE('',*,*,#6190,.T.);
#8226=ORIENTED_EDGE('',*,*,#6191,.F.);
#8227=ORIENTED_EDGE('',*,*,#6188,.F.);
#8228=ORIENTED_EDGE('',*,*,#6192,.F.);
#8229=ORIENTED_EDGE('',*,*,#6189,.F.);
#8230=ORIENTED_EDGE('',*,*,#6059,.F.);
#8231=ORIENTED_EDGE('',*,*,#6061,.T.);
#8232=ORIENTED_EDGE('',*,*,#6191,.T.);
#8233=ORIENTED_EDGE('',*,*,#6193,.T.);
#8234=ORIENTED_EDGE('',*,*,#6186,.T.);
#8235=ORIENTED_EDGE('',*,*,#6193,.F.);
#8236=ORIENTED_EDGE('',*,*,#6190,.F.);
#8237=ORIENTED_EDGE('',*,*,#6192,.T.);
#8238=ORIENTED_EDGE('',*,*,#6187,.T.);
#8239=ORIENTED_EDGE('',*,*,#5982,.T.);
#8240=ORIENTED_EDGE('',*,*,#6194,.F.);
#8241=ORIENTED_EDGE('',*,*,#6195,.F.);
#8242=ORIENTED_EDGE('',*,*,#6196,.T.);
#8243=ORIENTED_EDGE('',*,*,#5984,.T.);
#8244=ORIENTED_EDGE('',*,*,#6197,.T.);
#8245=ORIENTED_EDGE('',*,*,#6198,.T.);
#8246=ORIENTED_EDGE('',*,*,#6199,.F.);
#8247=ORIENTED_EDGE('',*,*,#6196,.F.);
#8248=ORIENTED_EDGE('',*,*,#6200,.F.);
#8249=ORIENTED_EDGE('',*,*,#6197,.F.);
#8250=ORIENTED_EDGE('',*,*,#5983,.F.);
#8251=ORIENTED_EDGE('',*,*,#5985,.T.);
#8252=ORIENTED_EDGE('',*,*,#6199,.T.);
#8253=ORIENTED_EDGE('',*,*,#6201,.T.);
#8254=ORIENTED_EDGE('',*,*,#6194,.T.);
#8255=ORIENTED_EDGE('',*,*,#6201,.F.);
#8256=ORIENTED_EDGE('',*,*,#6198,.F.);
#8257=ORIENTED_EDGE('',*,*,#6200,.T.);
#8258=ORIENTED_EDGE('',*,*,#6195,.T.);
#8259=ORIENTED_EDGE('',*,*,#5986,.T.);
#8260=ORIENTED_EDGE('',*,*,#6202,.F.);
#8261=ORIENTED_EDGE('',*,*,#6203,.F.);
#8262=ORIENTED_EDGE('',*,*,#6204,.T.);
#8263=ORIENTED_EDGE('',*,*,#5988,.T.);
#8264=ORIENTED_EDGE('',*,*,#6205,.T.);
#8265=ORIENTED_EDGE('',*,*,#6206,.T.);
#8266=ORIENTED_EDGE('',*,*,#6207,.F.);
#8267=ORIENTED_EDGE('',*,*,#6204,.F.);
#8268=ORIENTED_EDGE('',*,*,#6208,.F.);
#8269=ORIENTED_EDGE('',*,*,#6205,.F.);
#8270=ORIENTED_EDGE('',*,*,#5987,.F.);
#8271=ORIENTED_EDGE('',*,*,#5989,.T.);
#8272=ORIENTED_EDGE('',*,*,#6207,.T.);
#8273=ORIENTED_EDGE('',*,*,#6209,.T.);
#8274=ORIENTED_EDGE('',*,*,#6202,.T.);
#8275=ORIENTED_EDGE('',*,*,#6209,.F.);
#8276=ORIENTED_EDGE('',*,*,#6206,.F.);
#8277=ORIENTED_EDGE('',*,*,#6208,.T.);
#8278=ORIENTED_EDGE('',*,*,#6203,.T.);
#8279=ORIENTED_EDGE('',*,*,#5990,.T.);
#8280=ORIENTED_EDGE('',*,*,#6210,.F.);
#8281=ORIENTED_EDGE('',*,*,#6211,.F.);
#8282=ORIENTED_EDGE('',*,*,#6212,.T.);
#8283=ORIENTED_EDGE('',*,*,#5992,.T.);
#8284=ORIENTED_EDGE('',*,*,#6213,.T.);
#8285=ORIENTED_EDGE('',*,*,#6214,.T.);
#8286=ORIENTED_EDGE('',*,*,#6215,.F.);
#8287=ORIENTED_EDGE('',*,*,#6212,.F.);
#8288=ORIENTED_EDGE('',*,*,#6216,.F.);
#8289=ORIENTED_EDGE('',*,*,#6213,.F.);
#8290=ORIENTED_EDGE('',*,*,#5991,.F.);
#8291=ORIENTED_EDGE('',*,*,#5993,.T.);
#8292=ORIENTED_EDGE('',*,*,#6215,.T.);
#8293=ORIENTED_EDGE('',*,*,#6217,.T.);
#8294=ORIENTED_EDGE('',*,*,#6210,.T.);
#8295=ORIENTED_EDGE('',*,*,#6217,.F.);
#8296=ORIENTED_EDGE('',*,*,#6214,.F.);
#8297=ORIENTED_EDGE('',*,*,#6216,.T.);
#8298=ORIENTED_EDGE('',*,*,#6211,.T.);
#8299=ORIENTED_EDGE('',*,*,#5994,.T.);
#8300=ORIENTED_EDGE('',*,*,#6218,.F.);
#8301=ORIENTED_EDGE('',*,*,#6219,.F.);
#8302=ORIENTED_EDGE('',*,*,#6220,.T.);
#8303=ORIENTED_EDGE('',*,*,#5996,.T.);
#8304=ORIENTED_EDGE('',*,*,#6221,.T.);
#8305=ORIENTED_EDGE('',*,*,#6222,.T.);
#8306=ORIENTED_EDGE('',*,*,#6223,.F.);
#8307=ORIENTED_EDGE('',*,*,#6220,.F.);
#8308=ORIENTED_EDGE('',*,*,#6224,.F.);
#8309=ORIENTED_EDGE('',*,*,#6221,.F.);
#8310=ORIENTED_EDGE('',*,*,#5995,.F.);
#8311=ORIENTED_EDGE('',*,*,#5997,.T.);
#8312=ORIENTED_EDGE('',*,*,#6223,.T.);
#8313=ORIENTED_EDGE('',*,*,#6225,.T.);
#8314=ORIENTED_EDGE('',*,*,#6218,.T.);
#8315=ORIENTED_EDGE('',*,*,#6225,.F.);
#8316=ORIENTED_EDGE('',*,*,#6222,.F.);
#8317=ORIENTED_EDGE('',*,*,#6224,.T.);
#8318=ORIENTED_EDGE('',*,*,#6219,.T.);
#8319=ORIENTED_EDGE('',*,*,#5998,.T.);
#8320=ORIENTED_EDGE('',*,*,#6226,.F.);
#8321=ORIENTED_EDGE('',*,*,#6227,.F.);
#8322=ORIENTED_EDGE('',*,*,#6228,.T.);
#8323=ORIENTED_EDGE('',*,*,#6000,.T.);
#8324=ORIENTED_EDGE('',*,*,#6229,.T.);
#8325=ORIENTED_EDGE('',*,*,#6230,.T.);
#8326=ORIENTED_EDGE('',*,*,#6231,.F.);
#8327=ORIENTED_EDGE('',*,*,#6228,.F.);
#8328=ORIENTED_EDGE('',*,*,#6232,.F.);
#8329=ORIENTED_EDGE('',*,*,#6229,.F.);
#8330=ORIENTED_EDGE('',*,*,#5999,.F.);
#8331=ORIENTED_EDGE('',*,*,#6001,.T.);
#8332=ORIENTED_EDGE('',*,*,#6231,.T.);
#8333=ORIENTED_EDGE('',*,*,#6233,.T.);
#8334=ORIENTED_EDGE('',*,*,#6226,.T.);
#8335=ORIENTED_EDGE('',*,*,#6233,.F.);
#8336=ORIENTED_EDGE('',*,*,#6230,.F.);
#8337=ORIENTED_EDGE('',*,*,#6232,.T.);
#8338=ORIENTED_EDGE('',*,*,#6227,.T.);
#8339=ORIENTED_EDGE('',*,*,#6002,.T.);
#8340=ORIENTED_EDGE('',*,*,#6234,.F.);
#8341=ORIENTED_EDGE('',*,*,#6235,.F.);
#8342=ORIENTED_EDGE('',*,*,#6236,.T.);
#8343=ORIENTED_EDGE('',*,*,#6004,.T.);
#8344=ORIENTED_EDGE('',*,*,#6237,.T.);
#8345=ORIENTED_EDGE('',*,*,#6238,.T.);
#8346=ORIENTED_EDGE('',*,*,#6239,.F.);
#8347=ORIENTED_EDGE('',*,*,#6236,.F.);
#8348=ORIENTED_EDGE('',*,*,#6240,.F.);
#8349=ORIENTED_EDGE('',*,*,#6237,.F.);
#8350=ORIENTED_EDGE('',*,*,#6003,.F.);
#8351=ORIENTED_EDGE('',*,*,#6005,.T.);
#8352=ORIENTED_EDGE('',*,*,#6239,.T.);
#8353=ORIENTED_EDGE('',*,*,#6241,.T.);
#8354=ORIENTED_EDGE('',*,*,#6234,.T.);
#8355=ORIENTED_EDGE('',*,*,#6241,.F.);
#8356=ORIENTED_EDGE('',*,*,#6238,.F.);
#8357=ORIENTED_EDGE('',*,*,#6240,.T.);
#8358=ORIENTED_EDGE('',*,*,#6235,.T.);
#8359=ORIENTED_EDGE('',*,*,#6006,.T.);
#8360=ORIENTED_EDGE('',*,*,#6242,.F.);
#8361=ORIENTED_EDGE('',*,*,#6243,.F.);
#8362=ORIENTED_EDGE('',*,*,#6244,.T.);
#8363=ORIENTED_EDGE('',*,*,#6008,.T.);
#8364=ORIENTED_EDGE('',*,*,#6245,.T.);
#8365=ORIENTED_EDGE('',*,*,#6246,.T.);
#8366=ORIENTED_EDGE('',*,*,#6247,.F.);
#8367=ORIENTED_EDGE('',*,*,#6244,.F.);
#8368=ORIENTED_EDGE('',*,*,#6248,.F.);
#8369=ORIENTED_EDGE('',*,*,#6245,.F.);
#8370=ORIENTED_EDGE('',*,*,#6007,.F.);
#8371=ORIENTED_EDGE('',*,*,#6009,.T.);
#8372=ORIENTED_EDGE('',*,*,#6247,.T.);
#8373=ORIENTED_EDGE('',*,*,#6249,.T.);
#8374=ORIENTED_EDGE('',*,*,#6242,.T.);
#8375=ORIENTED_EDGE('',*,*,#6249,.F.);
#8376=ORIENTED_EDGE('',*,*,#6246,.F.);
#8377=ORIENTED_EDGE('',*,*,#6248,.T.);
#8378=ORIENTED_EDGE('',*,*,#6243,.T.);
#8379=ORIENTED_EDGE('',*,*,#6010,.T.);
#8380=ORIENTED_EDGE('',*,*,#6250,.F.);
#8381=ORIENTED_EDGE('',*,*,#6251,.F.);
#8382=ORIENTED_EDGE('',*,*,#6252,.T.);
#8383=ORIENTED_EDGE('',*,*,#6012,.T.);
#8384=ORIENTED_EDGE('',*,*,#6253,.T.);
#8385=ORIENTED_EDGE('',*,*,#6254,.T.);
#8386=ORIENTED_EDGE('',*,*,#6255,.F.);
#8387=ORIENTED_EDGE('',*,*,#6252,.F.);
#8388=ORIENTED_EDGE('',*,*,#6256,.F.);
#8389=ORIENTED_EDGE('',*,*,#6253,.F.);
#8390=ORIENTED_EDGE('',*,*,#6011,.F.);
#8391=ORIENTED_EDGE('',*,*,#6013,.T.);
#8392=ORIENTED_EDGE('',*,*,#6255,.T.);
#8393=ORIENTED_EDGE('',*,*,#6257,.T.);
#8394=ORIENTED_EDGE('',*,*,#6250,.T.);
#8395=ORIENTED_EDGE('',*,*,#6257,.F.);
#8396=ORIENTED_EDGE('',*,*,#6254,.F.);
#8397=ORIENTED_EDGE('',*,*,#6256,.T.);
#8398=ORIENTED_EDGE('',*,*,#6251,.T.);
#8399=ORIENTED_EDGE('',*,*,#6014,.T.);
#8400=ORIENTED_EDGE('',*,*,#6258,.F.);
#8401=ORIENTED_EDGE('',*,*,#6259,.F.);
#8402=ORIENTED_EDGE('',*,*,#6260,.T.);
#8403=ORIENTED_EDGE('',*,*,#6016,.T.);
#8404=ORIENTED_EDGE('',*,*,#6261,.T.);
#8405=ORIENTED_EDGE('',*,*,#6262,.T.);
#8406=ORIENTED_EDGE('',*,*,#6263,.F.);
#8407=ORIENTED_EDGE('',*,*,#6260,.F.);
#8408=ORIENTED_EDGE('',*,*,#6264,.F.);
#8409=ORIENTED_EDGE('',*,*,#6261,.F.);
#8410=ORIENTED_EDGE('',*,*,#6015,.F.);
#8411=ORIENTED_EDGE('',*,*,#6017,.T.);
#8412=ORIENTED_EDGE('',*,*,#6263,.T.);
#8413=ORIENTED_EDGE('',*,*,#6265,.T.);
#8414=ORIENTED_EDGE('',*,*,#6258,.T.);
#8415=ORIENTED_EDGE('',*,*,#6265,.F.);
#8416=ORIENTED_EDGE('',*,*,#6262,.F.);
#8417=ORIENTED_EDGE('',*,*,#6264,.T.);
#8418=ORIENTED_EDGE('',*,*,#6259,.T.);
#8419=ORIENTED_EDGE('',*,*,#6018,.T.);
#8420=ORIENTED_EDGE('',*,*,#6266,.F.);
#8421=ORIENTED_EDGE('',*,*,#6267,.F.);
#8422=ORIENTED_EDGE('',*,*,#6268,.T.);
#8423=ORIENTED_EDGE('',*,*,#6020,.T.);
#8424=ORIENTED_EDGE('',*,*,#6269,.T.);
#8425=ORIENTED_EDGE('',*,*,#6270,.T.);
#8426=ORIENTED_EDGE('',*,*,#6271,.F.);
#8427=ORIENTED_EDGE('',*,*,#6268,.F.);
#8428=ORIENTED_EDGE('',*,*,#6272,.F.);
#8429=ORIENTED_EDGE('',*,*,#6269,.F.);
#8430=ORIENTED_EDGE('',*,*,#6019,.F.);
#8431=ORIENTED_EDGE('',*,*,#6021,.T.);
#8432=ORIENTED_EDGE('',*,*,#6271,.T.);
#8433=ORIENTED_EDGE('',*,*,#6273,.T.);
#8434=ORIENTED_EDGE('',*,*,#6266,.T.);
#8435=ORIENTED_EDGE('',*,*,#6273,.F.);
#8436=ORIENTED_EDGE('',*,*,#6270,.F.);
#8437=ORIENTED_EDGE('',*,*,#6272,.T.);
#8438=ORIENTED_EDGE('',*,*,#6267,.T.);
#8439=ORIENTED_EDGE('',*,*,#6022,.T.);
#8440=ORIENTED_EDGE('',*,*,#6274,.F.);
#8441=ORIENTED_EDGE('',*,*,#6275,.F.);
#8442=ORIENTED_EDGE('',*,*,#6276,.T.);
#8443=ORIENTED_EDGE('',*,*,#6024,.T.);
#8444=ORIENTED_EDGE('',*,*,#6277,.T.);
#8445=ORIENTED_EDGE('',*,*,#6278,.T.);
#8446=ORIENTED_EDGE('',*,*,#6279,.F.);
#8447=ORIENTED_EDGE('',*,*,#6276,.F.);
#8448=ORIENTED_EDGE('',*,*,#6280,.F.);
#8449=ORIENTED_EDGE('',*,*,#6277,.F.);
#8450=ORIENTED_EDGE('',*,*,#6023,.F.);
#8451=ORIENTED_EDGE('',*,*,#6025,.T.);
#8452=ORIENTED_EDGE('',*,*,#6279,.T.);
#8453=ORIENTED_EDGE('',*,*,#6281,.T.);
#8454=ORIENTED_EDGE('',*,*,#6274,.T.);
#8455=ORIENTED_EDGE('',*,*,#6281,.F.);
#8456=ORIENTED_EDGE('',*,*,#6278,.F.);
#8457=ORIENTED_EDGE('',*,*,#6280,.T.);
#8458=ORIENTED_EDGE('',*,*,#6275,.T.);
#8459=ORIENTED_EDGE('',*,*,#6026,.T.);
#8460=ORIENTED_EDGE('',*,*,#6282,.F.);
#8461=ORIENTED_EDGE('',*,*,#6283,.F.);
#8462=ORIENTED_EDGE('',*,*,#6284,.T.);
#8463=ORIENTED_EDGE('',*,*,#6028,.T.);
#8464=ORIENTED_EDGE('',*,*,#6285,.T.);
#8465=ORIENTED_EDGE('',*,*,#6286,.T.);
#8466=ORIENTED_EDGE('',*,*,#6287,.F.);
#8467=ORIENTED_EDGE('',*,*,#6284,.F.);
#8468=ORIENTED_EDGE('',*,*,#6288,.F.);
#8469=ORIENTED_EDGE('',*,*,#6285,.F.);
#8470=ORIENTED_EDGE('',*,*,#6027,.F.);
#8471=ORIENTED_EDGE('',*,*,#6029,.T.);
#8472=ORIENTED_EDGE('',*,*,#6287,.T.);
#8473=ORIENTED_EDGE('',*,*,#6289,.T.);
#8474=ORIENTED_EDGE('',*,*,#6282,.T.);
#8475=ORIENTED_EDGE('',*,*,#6289,.F.);
#8476=ORIENTED_EDGE('',*,*,#6286,.F.);
#8477=ORIENTED_EDGE('',*,*,#6288,.T.);
#8478=ORIENTED_EDGE('',*,*,#6283,.T.);
#8479=ORIENTED_EDGE('',*,*,#6030,.T.);
#8480=ORIENTED_EDGE('',*,*,#6290,.F.);
#8481=ORIENTED_EDGE('',*,*,#6291,.F.);
#8482=ORIENTED_EDGE('',*,*,#6292,.T.);
#8483=ORIENTED_EDGE('',*,*,#6032,.T.);
#8484=ORIENTED_EDGE('',*,*,#6293,.T.);
#8485=ORIENTED_EDGE('',*,*,#6294,.T.);
#8486=ORIENTED_EDGE('',*,*,#6295,.F.);
#8487=ORIENTED_EDGE('',*,*,#6292,.F.);
#8488=ORIENTED_EDGE('',*,*,#6296,.F.);
#8489=ORIENTED_EDGE('',*,*,#6293,.F.);
#8490=ORIENTED_EDGE('',*,*,#6031,.F.);
#8491=ORIENTED_EDGE('',*,*,#6033,.T.);
#8492=ORIENTED_EDGE('',*,*,#6295,.T.);
#8493=ORIENTED_EDGE('',*,*,#6297,.T.);
#8494=ORIENTED_EDGE('',*,*,#6290,.T.);
#8495=ORIENTED_EDGE('',*,*,#6297,.F.);
#8496=ORIENTED_EDGE('',*,*,#6294,.F.);
#8497=ORIENTED_EDGE('',*,*,#6296,.T.);
#8498=ORIENTED_EDGE('',*,*,#6291,.T.);
#8499=ORIENTED_EDGE('',*,*,#6034,.T.);
#8500=ORIENTED_EDGE('',*,*,#6298,.F.);
#8501=ORIENTED_EDGE('',*,*,#6299,.F.);
#8502=ORIENTED_EDGE('',*,*,#6300,.T.);
#8503=ORIENTED_EDGE('',*,*,#6036,.T.);
#8504=ORIENTED_EDGE('',*,*,#6301,.T.);
#8505=ORIENTED_EDGE('',*,*,#6302,.T.);
#8506=ORIENTED_EDGE('',*,*,#6303,.F.);
#8507=ORIENTED_EDGE('',*,*,#6300,.F.);
#8508=ORIENTED_EDGE('',*,*,#6304,.F.);
#8509=ORIENTED_EDGE('',*,*,#6301,.F.);
#8510=ORIENTED_EDGE('',*,*,#6035,.F.);
#8511=ORIENTED_EDGE('',*,*,#6037,.T.);
#8512=ORIENTED_EDGE('',*,*,#6303,.T.);
#8513=ORIENTED_EDGE('',*,*,#6305,.T.);
#8514=ORIENTED_EDGE('',*,*,#6298,.T.);
#8515=ORIENTED_EDGE('',*,*,#6305,.F.);
#8516=ORIENTED_EDGE('',*,*,#6302,.F.);
#8517=ORIENTED_EDGE('',*,*,#6304,.T.);
#8518=ORIENTED_EDGE('',*,*,#6299,.T.);
#8519=ORIENTED_EDGE('',*,*,#6038,.T.);
#8520=ORIENTED_EDGE('',*,*,#6306,.F.);
#8521=ORIENTED_EDGE('',*,*,#6307,.F.);
#8522=ORIENTED_EDGE('',*,*,#6308,.T.);
#8523=ORIENTED_EDGE('',*,*,#6040,.T.);
#8524=ORIENTED_EDGE('',*,*,#6309,.T.);
#8525=ORIENTED_EDGE('',*,*,#6310,.T.);
#8526=ORIENTED_EDGE('',*,*,#6311,.F.);
#8527=ORIENTED_EDGE('',*,*,#6308,.F.);
#8528=ORIENTED_EDGE('',*,*,#6312,.F.);
#8529=ORIENTED_EDGE('',*,*,#6309,.F.);
#8530=ORIENTED_EDGE('',*,*,#6039,.F.);
#8531=ORIENTED_EDGE('',*,*,#6041,.T.);
#8532=ORIENTED_EDGE('',*,*,#6311,.T.);
#8533=ORIENTED_EDGE('',*,*,#6313,.T.);
#8534=ORIENTED_EDGE('',*,*,#6306,.T.);
#8535=ORIENTED_EDGE('',*,*,#6313,.F.);
#8536=ORIENTED_EDGE('',*,*,#6310,.F.);
#8537=ORIENTED_EDGE('',*,*,#6312,.T.);
#8538=ORIENTED_EDGE('',*,*,#6307,.T.);
#8539=ORIENTED_EDGE('',*,*,#6042,.T.);
#8540=ORIENTED_EDGE('',*,*,#6314,.F.);
#8541=ORIENTED_EDGE('',*,*,#6315,.F.);
#8542=ORIENTED_EDGE('',*,*,#6316,.T.);
#8543=ORIENTED_EDGE('',*,*,#6044,.T.);
#8544=ORIENTED_EDGE('',*,*,#6317,.T.);
#8545=ORIENTED_EDGE('',*,*,#6318,.T.);
#8546=ORIENTED_EDGE('',*,*,#6319,.F.);
#8547=ORIENTED_EDGE('',*,*,#6316,.F.);
#8548=ORIENTED_EDGE('',*,*,#6320,.F.);
#8549=ORIENTED_EDGE('',*,*,#6317,.F.);
#8550=ORIENTED_EDGE('',*,*,#6043,.F.);
#8551=ORIENTED_EDGE('',*,*,#6045,.T.);
#8552=ORIENTED_EDGE('',*,*,#6319,.T.);
#8553=ORIENTED_EDGE('',*,*,#6321,.T.);
#8554=ORIENTED_EDGE('',*,*,#6314,.T.);
#8555=ORIENTED_EDGE('',*,*,#6321,.F.);
#8556=ORIENTED_EDGE('',*,*,#6318,.F.);
#8557=ORIENTED_EDGE('',*,*,#6320,.T.);
#8558=ORIENTED_EDGE('',*,*,#6315,.T.);
#8559=ORIENTED_EDGE('',*,*,#6062,.T.);
#8560=ORIENTED_EDGE('',*,*,#6322,.F.);
#8561=ORIENTED_EDGE('',*,*,#6323,.F.);
#8562=ORIENTED_EDGE('',*,*,#6324,.T.);
#8563=ORIENTED_EDGE('',*,*,#6064,.T.);
#8564=ORIENTED_EDGE('',*,*,#6325,.T.);
#8565=ORIENTED_EDGE('',*,*,#6326,.T.);
#8566=ORIENTED_EDGE('',*,*,#6327,.F.);
#8567=ORIENTED_EDGE('',*,*,#6324,.F.);
#8568=ORIENTED_EDGE('',*,*,#6328,.F.);
#8569=ORIENTED_EDGE('',*,*,#6325,.F.);
#8570=ORIENTED_EDGE('',*,*,#6063,.F.);
#8571=ORIENTED_EDGE('',*,*,#6065,.T.);
#8572=ORIENTED_EDGE('',*,*,#6327,.T.);
#8573=ORIENTED_EDGE('',*,*,#6329,.T.);
#8574=ORIENTED_EDGE('',*,*,#6322,.T.);
#8575=ORIENTED_EDGE('',*,*,#6329,.F.);
#8576=ORIENTED_EDGE('',*,*,#6326,.F.);
#8577=ORIENTED_EDGE('',*,*,#6328,.T.);
#8578=ORIENTED_EDGE('',*,*,#6323,.T.);
#8579=ORIENTED_EDGE('',*,*,#6066,.T.);
#8580=ORIENTED_EDGE('',*,*,#6330,.F.);
#8581=ORIENTED_EDGE('',*,*,#6331,.F.);
#8582=ORIENTED_EDGE('',*,*,#6332,.T.);
#8583=ORIENTED_EDGE('',*,*,#6068,.T.);
#8584=ORIENTED_EDGE('',*,*,#6333,.T.);
#8585=ORIENTED_EDGE('',*,*,#6334,.T.);
#8586=ORIENTED_EDGE('',*,*,#6335,.F.);
#8587=ORIENTED_EDGE('',*,*,#6332,.F.);
#8588=ORIENTED_EDGE('',*,*,#6336,.F.);
#8589=ORIENTED_EDGE('',*,*,#6333,.F.);
#8590=ORIENTED_EDGE('',*,*,#6067,.F.);
#8591=ORIENTED_EDGE('',*,*,#6069,.T.);
#8592=ORIENTED_EDGE('',*,*,#6335,.T.);
#8593=ORIENTED_EDGE('',*,*,#6337,.T.);
#8594=ORIENTED_EDGE('',*,*,#6330,.T.);
#8595=ORIENTED_EDGE('',*,*,#6337,.F.);
#8596=ORIENTED_EDGE('',*,*,#6334,.F.);
#8597=ORIENTED_EDGE('',*,*,#6336,.T.);
#8598=ORIENTED_EDGE('',*,*,#6331,.T.);
#8599=ORIENTED_EDGE('',*,*,#6070,.T.);
#8600=ORIENTED_EDGE('',*,*,#6338,.F.);
#8601=ORIENTED_EDGE('',*,*,#6339,.F.);
#8602=ORIENTED_EDGE('',*,*,#6340,.T.);
#8603=ORIENTED_EDGE('',*,*,#6072,.T.);
#8604=ORIENTED_EDGE('',*,*,#6341,.T.);
#8605=ORIENTED_EDGE('',*,*,#6342,.T.);
#8606=ORIENTED_EDGE('',*,*,#6343,.F.);
#8607=ORIENTED_EDGE('',*,*,#6340,.F.);
#8608=ORIENTED_EDGE('',*,*,#6344,.F.);
#8609=ORIENTED_EDGE('',*,*,#6341,.F.);
#8610=ORIENTED_EDGE('',*,*,#6071,.F.);
#8611=ORIENTED_EDGE('',*,*,#6073,.T.);
#8612=ORIENTED_EDGE('',*,*,#6343,.T.);
#8613=ORIENTED_EDGE('',*,*,#6345,.T.);
#8614=ORIENTED_EDGE('',*,*,#6338,.T.);
#8615=ORIENTED_EDGE('',*,*,#6345,.F.);
#8616=ORIENTED_EDGE('',*,*,#6342,.F.);
#8617=ORIENTED_EDGE('',*,*,#6344,.T.);
#8618=ORIENTED_EDGE('',*,*,#6339,.T.);
#8619=ORIENTED_EDGE('',*,*,#6074,.T.);
#8620=ORIENTED_EDGE('',*,*,#6346,.F.);
#8621=ORIENTED_EDGE('',*,*,#6347,.F.);
#8622=ORIENTED_EDGE('',*,*,#6348,.T.);
#8623=ORIENTED_EDGE('',*,*,#6076,.T.);
#8624=ORIENTED_EDGE('',*,*,#6349,.T.);
#8625=ORIENTED_EDGE('',*,*,#6350,.T.);
#8626=ORIENTED_EDGE('',*,*,#6351,.F.);
#8627=ORIENTED_EDGE('',*,*,#6348,.F.);
#8628=ORIENTED_EDGE('',*,*,#6352,.F.);
#8629=ORIENTED_EDGE('',*,*,#6349,.F.);
#8630=ORIENTED_EDGE('',*,*,#6075,.F.);
#8631=ORIENTED_EDGE('',*,*,#6077,.T.);
#8632=ORIENTED_EDGE('',*,*,#6351,.T.);
#8633=ORIENTED_EDGE('',*,*,#6353,.T.);
#8634=ORIENTED_EDGE('',*,*,#6346,.T.);
#8635=ORIENTED_EDGE('',*,*,#6353,.F.);
#8636=ORIENTED_EDGE('',*,*,#6350,.F.);
#8637=ORIENTED_EDGE('',*,*,#6352,.T.);
#8638=ORIENTED_EDGE('',*,*,#6347,.T.);
#8639=ORIENTED_EDGE('',*,*,#6078,.T.);
#8640=ORIENTED_EDGE('',*,*,#6354,.F.);
#8641=ORIENTED_EDGE('',*,*,#6355,.F.);
#8642=ORIENTED_EDGE('',*,*,#6356,.T.);
#8643=ORIENTED_EDGE('',*,*,#6080,.T.);
#8644=ORIENTED_EDGE('',*,*,#6357,.T.);
#8645=ORIENTED_EDGE('',*,*,#6358,.T.);
#8646=ORIENTED_EDGE('',*,*,#6359,.F.);
#8647=ORIENTED_EDGE('',*,*,#6356,.F.);
#8648=ORIENTED_EDGE('',*,*,#6360,.F.);
#8649=ORIENTED_EDGE('',*,*,#6357,.F.);
#8650=ORIENTED_EDGE('',*,*,#6079,.F.);
#8651=ORIENTED_EDGE('',*,*,#6081,.T.);
#8652=ORIENTED_EDGE('',*,*,#6359,.T.);
#8653=ORIENTED_EDGE('',*,*,#6361,.T.);
#8654=ORIENTED_EDGE('',*,*,#6354,.T.);
#8655=ORIENTED_EDGE('',*,*,#6361,.F.);
#8656=ORIENTED_EDGE('',*,*,#6358,.F.);
#8657=ORIENTED_EDGE('',*,*,#6360,.T.);
#8658=ORIENTED_EDGE('',*,*,#6355,.T.);
#8659=ORIENTED_EDGE('',*,*,#6082,.T.);
#8660=ORIENTED_EDGE('',*,*,#6362,.F.);
#8661=ORIENTED_EDGE('',*,*,#6363,.F.);
#8662=ORIENTED_EDGE('',*,*,#6364,.T.);
#8663=ORIENTED_EDGE('',*,*,#6084,.T.);
#8664=ORIENTED_EDGE('',*,*,#6365,.T.);
#8665=ORIENTED_EDGE('',*,*,#6366,.T.);
#8666=ORIENTED_EDGE('',*,*,#6367,.F.);
#8667=ORIENTED_EDGE('',*,*,#6364,.F.);
#8668=ORIENTED_EDGE('',*,*,#6368,.F.);
#8669=ORIENTED_EDGE('',*,*,#6365,.F.);
#8670=ORIENTED_EDGE('',*,*,#6083,.F.);
#8671=ORIENTED_EDGE('',*,*,#6085,.T.);
#8672=ORIENTED_EDGE('',*,*,#6367,.T.);
#8673=ORIENTED_EDGE('',*,*,#6369,.T.);
#8674=ORIENTED_EDGE('',*,*,#6362,.T.);
#8675=ORIENTED_EDGE('',*,*,#6369,.F.);
#8676=ORIENTED_EDGE('',*,*,#6366,.F.);
#8677=ORIENTED_EDGE('',*,*,#6368,.T.);
#8678=ORIENTED_EDGE('',*,*,#6363,.T.);
#8679=ORIENTED_EDGE('',*,*,#6086,.T.);
#8680=ORIENTED_EDGE('',*,*,#6370,.F.);
#8681=ORIENTED_EDGE('',*,*,#6371,.F.);
#8682=ORIENTED_EDGE('',*,*,#6372,.T.);
#8683=ORIENTED_EDGE('',*,*,#6088,.T.);
#8684=ORIENTED_EDGE('',*,*,#6373,.T.);
#8685=ORIENTED_EDGE('',*,*,#6374,.T.);
#8686=ORIENTED_EDGE('',*,*,#6375,.F.);
#8687=ORIENTED_EDGE('',*,*,#6372,.F.);
#8688=ORIENTED_EDGE('',*,*,#6376,.F.);
#8689=ORIENTED_EDGE('',*,*,#6373,.F.);
#8690=ORIENTED_EDGE('',*,*,#6087,.F.);
#8691=ORIENTED_EDGE('',*,*,#6089,.T.);
#8692=ORIENTED_EDGE('',*,*,#6375,.T.);
#8693=ORIENTED_EDGE('',*,*,#6377,.T.);
#8694=ORIENTED_EDGE('',*,*,#6370,.T.);
#8695=ORIENTED_EDGE('',*,*,#6377,.F.);
#8696=ORIENTED_EDGE('',*,*,#6374,.F.);
#8697=ORIENTED_EDGE('',*,*,#6376,.T.);
#8698=ORIENTED_EDGE('',*,*,#6371,.T.);
#8699=ORIENTED_EDGE('',*,*,#6090,.T.);
#8700=ORIENTED_EDGE('',*,*,#6378,.F.);
#8701=ORIENTED_EDGE('',*,*,#6379,.F.);
#8702=ORIENTED_EDGE('',*,*,#6380,.T.);
#8703=ORIENTED_EDGE('',*,*,#6092,.T.);
#8704=ORIENTED_EDGE('',*,*,#6381,.T.);
#8705=ORIENTED_EDGE('',*,*,#6382,.T.);
#8706=ORIENTED_EDGE('',*,*,#6383,.F.);
#8707=ORIENTED_EDGE('',*,*,#6380,.F.);
#8708=ORIENTED_EDGE('',*,*,#6384,.F.);
#8709=ORIENTED_EDGE('',*,*,#6381,.F.);
#8710=ORIENTED_EDGE('',*,*,#6091,.F.);
#8711=ORIENTED_EDGE('',*,*,#6093,.T.);
#8712=ORIENTED_EDGE('',*,*,#6383,.T.);
#8713=ORIENTED_EDGE('',*,*,#6385,.T.);
#8714=ORIENTED_EDGE('',*,*,#6378,.T.);
#8715=ORIENTED_EDGE('',*,*,#6385,.F.);
#8716=ORIENTED_EDGE('',*,*,#6382,.F.);
#8717=ORIENTED_EDGE('',*,*,#6384,.T.);
#8718=ORIENTED_EDGE('',*,*,#6379,.T.);
#8719=ORIENTED_EDGE('',*,*,#6094,.T.);
#8720=ORIENTED_EDGE('',*,*,#6386,.F.);
#8721=ORIENTED_EDGE('',*,*,#6387,.F.);
#8722=ORIENTED_EDGE('',*,*,#6388,.T.);
#8723=ORIENTED_EDGE('',*,*,#6096,.T.);
#8724=ORIENTED_EDGE('',*,*,#6389,.T.);
#8725=ORIENTED_EDGE('',*,*,#6390,.T.);
#8726=ORIENTED_EDGE('',*,*,#6391,.F.);
#8727=ORIENTED_EDGE('',*,*,#6388,.F.);
#8728=ORIENTED_EDGE('',*,*,#6392,.F.);
#8729=ORIENTED_EDGE('',*,*,#6389,.F.);
#8730=ORIENTED_EDGE('',*,*,#6095,.F.);
#8731=ORIENTED_EDGE('',*,*,#6097,.T.);
#8732=ORIENTED_EDGE('',*,*,#6391,.T.);
#8733=ORIENTED_EDGE('',*,*,#6393,.T.);
#8734=ORIENTED_EDGE('',*,*,#6386,.T.);
#8735=ORIENTED_EDGE('',*,*,#6393,.F.);
#8736=ORIENTED_EDGE('',*,*,#6390,.F.);
#8737=ORIENTED_EDGE('',*,*,#6392,.T.);
#8738=ORIENTED_EDGE('',*,*,#6387,.T.);
#8739=ORIENTED_EDGE('',*,*,#6098,.T.);
#8740=ORIENTED_EDGE('',*,*,#6394,.F.);
#8741=ORIENTED_EDGE('',*,*,#6395,.F.);
#8742=ORIENTED_EDGE('',*,*,#6396,.T.);
#8743=ORIENTED_EDGE('',*,*,#6100,.T.);
#8744=ORIENTED_EDGE('',*,*,#6397,.T.);
#8745=ORIENTED_EDGE('',*,*,#6398,.T.);
#8746=ORIENTED_EDGE('',*,*,#6399,.F.);
#8747=ORIENTED_EDGE('',*,*,#6396,.F.);
#8748=ORIENTED_EDGE('',*,*,#6400,.F.);
#8749=ORIENTED_EDGE('',*,*,#6397,.F.);
#8750=ORIENTED_EDGE('',*,*,#6099,.F.);
#8751=ORIENTED_EDGE('',*,*,#6101,.T.);
#8752=ORIENTED_EDGE('',*,*,#6399,.T.);
#8753=ORIENTED_EDGE('',*,*,#6401,.T.);
#8754=ORIENTED_EDGE('',*,*,#6394,.T.);
#8755=ORIENTED_EDGE('',*,*,#6401,.F.);
#8756=ORIENTED_EDGE('',*,*,#6398,.F.);
#8757=ORIENTED_EDGE('',*,*,#6400,.T.);
#8758=ORIENTED_EDGE('',*,*,#6395,.T.);
#8759=ORIENTED_EDGE('',*,*,#6102,.T.);
#8760=ORIENTED_EDGE('',*,*,#6402,.F.);
#8761=ORIENTED_EDGE('',*,*,#6403,.F.);
#8762=ORIENTED_EDGE('',*,*,#6404,.T.);
#8763=ORIENTED_EDGE('',*,*,#6104,.T.);
#8764=ORIENTED_EDGE('',*,*,#6405,.T.);
#8765=ORIENTED_EDGE('',*,*,#6406,.T.);
#8766=ORIENTED_EDGE('',*,*,#6407,.F.);
#8767=ORIENTED_EDGE('',*,*,#6404,.F.);
#8768=ORIENTED_EDGE('',*,*,#6408,.F.);
#8769=ORIENTED_EDGE('',*,*,#6405,.F.);
#8770=ORIENTED_EDGE('',*,*,#6103,.F.);
#8771=ORIENTED_EDGE('',*,*,#6105,.T.);
#8772=ORIENTED_EDGE('',*,*,#6407,.T.);
#8773=ORIENTED_EDGE('',*,*,#6409,.T.);
#8774=ORIENTED_EDGE('',*,*,#6402,.T.);
#8775=ORIENTED_EDGE('',*,*,#6409,.F.);
#8776=ORIENTED_EDGE('',*,*,#6406,.F.);
#8777=ORIENTED_EDGE('',*,*,#6408,.T.);
#8778=ORIENTED_EDGE('',*,*,#6403,.T.);
#8779=ORIENTED_EDGE('',*,*,#6106,.T.);
#8780=ORIENTED_EDGE('',*,*,#6410,.F.);
#8781=ORIENTED_EDGE('',*,*,#6411,.F.);
#8782=ORIENTED_EDGE('',*,*,#6412,.T.);
#8783=ORIENTED_EDGE('',*,*,#6108,.T.);
#8784=ORIENTED_EDGE('',*,*,#6413,.T.);
#8785=ORIENTED_EDGE('',*,*,#6414,.T.);
#8786=ORIENTED_EDGE('',*,*,#6415,.F.);
#8787=ORIENTED_EDGE('',*,*,#6412,.F.);
#8788=ORIENTED_EDGE('',*,*,#6416,.F.);
#8789=ORIENTED_EDGE('',*,*,#6413,.F.);
#8790=ORIENTED_EDGE('',*,*,#6107,.F.);
#8791=ORIENTED_EDGE('',*,*,#6109,.T.);
#8792=ORIENTED_EDGE('',*,*,#6415,.T.);
#8793=ORIENTED_EDGE('',*,*,#6417,.T.);
#8794=ORIENTED_EDGE('',*,*,#6410,.T.);
#8795=ORIENTED_EDGE('',*,*,#6417,.F.);
#8796=ORIENTED_EDGE('',*,*,#6414,.F.);
#8797=ORIENTED_EDGE('',*,*,#6416,.T.);
#8798=ORIENTED_EDGE('',*,*,#6411,.T.);
#8799=ORIENTED_EDGE('',*,*,#6110,.T.);
#8800=ORIENTED_EDGE('',*,*,#6418,.F.);
#8801=ORIENTED_EDGE('',*,*,#6419,.F.);
#8802=ORIENTED_EDGE('',*,*,#6420,.T.);
#8803=ORIENTED_EDGE('',*,*,#6112,.T.);
#8804=ORIENTED_EDGE('',*,*,#6421,.T.);
#8805=ORIENTED_EDGE('',*,*,#6422,.T.);
#8806=ORIENTED_EDGE('',*,*,#6423,.F.);
#8807=ORIENTED_EDGE('',*,*,#6420,.F.);
#8808=ORIENTED_EDGE('',*,*,#6424,.F.);
#8809=ORIENTED_EDGE('',*,*,#6421,.F.);
#8810=ORIENTED_EDGE('',*,*,#6111,.F.);
#8811=ORIENTED_EDGE('',*,*,#6113,.T.);
#8812=ORIENTED_EDGE('',*,*,#6423,.T.);
#8813=ORIENTED_EDGE('',*,*,#6425,.T.);
#8814=ORIENTED_EDGE('',*,*,#6418,.T.);
#8815=ORIENTED_EDGE('',*,*,#6425,.F.);
#8816=ORIENTED_EDGE('',*,*,#6422,.F.);
#8817=ORIENTED_EDGE('',*,*,#6424,.T.);
#8818=ORIENTED_EDGE('',*,*,#6419,.T.);
#8819=ORIENTED_EDGE('',*,*,#6114,.T.);
#8820=ORIENTED_EDGE('',*,*,#6426,.F.);
#8821=ORIENTED_EDGE('',*,*,#6427,.F.);
#8822=ORIENTED_EDGE('',*,*,#6428,.T.);
#8823=ORIENTED_EDGE('',*,*,#6116,.T.);
#8824=ORIENTED_EDGE('',*,*,#6429,.T.);
#8825=ORIENTED_EDGE('',*,*,#6430,.T.);
#8826=ORIENTED_EDGE('',*,*,#6431,.F.);
#8827=ORIENTED_EDGE('',*,*,#6428,.F.);
#8828=ORIENTED_EDGE('',*,*,#6432,.F.);
#8829=ORIENTED_EDGE('',*,*,#6429,.F.);
#8830=ORIENTED_EDGE('',*,*,#6115,.F.);
#8831=ORIENTED_EDGE('',*,*,#6117,.T.);
#8832=ORIENTED_EDGE('',*,*,#6431,.T.);
#8833=ORIENTED_EDGE('',*,*,#6433,.T.);
#8834=ORIENTED_EDGE('',*,*,#6426,.T.);
#8835=ORIENTED_EDGE('',*,*,#6433,.F.);
#8836=ORIENTED_EDGE('',*,*,#6430,.F.);
#8837=ORIENTED_EDGE('',*,*,#6432,.T.);
#8838=ORIENTED_EDGE('',*,*,#6427,.T.);
#8839=ORIENTED_EDGE('',*,*,#6118,.T.);
#8840=ORIENTED_EDGE('',*,*,#6434,.F.);
#8841=ORIENTED_EDGE('',*,*,#6435,.F.);
#8842=ORIENTED_EDGE('',*,*,#6436,.T.);
#8843=ORIENTED_EDGE('',*,*,#6120,.T.);
#8844=ORIENTED_EDGE('',*,*,#6437,.T.);
#8845=ORIENTED_EDGE('',*,*,#6438,.T.);
#8846=ORIENTED_EDGE('',*,*,#6439,.F.);
#8847=ORIENTED_EDGE('',*,*,#6436,.F.);
#8848=ORIENTED_EDGE('',*,*,#6440,.F.);
#8849=ORIENTED_EDGE('',*,*,#6437,.F.);
#8850=ORIENTED_EDGE('',*,*,#6119,.F.);
#8851=ORIENTED_EDGE('',*,*,#6121,.T.);
#8852=ORIENTED_EDGE('',*,*,#6439,.T.);
#8853=ORIENTED_EDGE('',*,*,#6441,.T.);
#8854=ORIENTED_EDGE('',*,*,#6434,.T.);
#8855=ORIENTED_EDGE('',*,*,#6441,.F.);
#8856=ORIENTED_EDGE('',*,*,#6438,.F.);
#8857=ORIENTED_EDGE('',*,*,#6440,.T.);
#8858=ORIENTED_EDGE('',*,*,#6435,.T.);
#8859=ORIENTED_EDGE('',*,*,#6442,.T.);
#8860=ORIENTED_EDGE('',*,*,#6443,.T.);
#8861=ORIENTED_EDGE('',*,*,#6444,.F.);
#8862=ORIENTED_EDGE('',*,*,#6443,.F.);
#8863=ORIENTED_EDGE('',*,*,#6445,.T.);
#8864=ORIENTED_EDGE('',*,*,#6446,.T.);
#8865=ORIENTED_EDGE('',*,*,#6447,.F.);
#8866=ORIENTED_EDGE('',*,*,#6446,.F.);
#8867=ORIENTED_EDGE('',*,*,#6448,.T.);
#8868=ORIENTED_EDGE('',*,*,#6449,.T.);
#8869=ORIENTED_EDGE('',*,*,#6450,.T.);
#8870=ORIENTED_EDGE('',*,*,#6451,.T.);
#8871=ORIENTED_EDGE('',*,*,#6452,.T.);
#8872=ORIENTED_EDGE('',*,*,#6453,.T.);
#8873=ORIENTED_EDGE('',*,*,#6454,.T.);
#8874=ORIENTED_EDGE('',*,*,#6455,.T.);
#8875=ORIENTED_EDGE('',*,*,#6456,.T.);
#8876=ORIENTED_EDGE('',*,*,#6457,.T.);
#8877=ORIENTED_EDGE('',*,*,#6458,.T.);
#8878=ORIENTED_EDGE('',*,*,#6459,.T.);
#8879=ORIENTED_EDGE('',*,*,#6460,.T.);
#8880=ORIENTED_EDGE('',*,*,#6461,.T.);
#8881=ORIENTED_EDGE('',*,*,#6442,.F.);
#8882=ORIENTED_EDGE('',*,*,#6445,.F.);
#8883=ORIENTED_EDGE('',*,*,#6462,.F.);
#8884=ORIENTED_EDGE('',*,*,#6463,.F.);
#8885=ORIENTED_EDGE('',*,*,#6464,.F.);
#8886=ORIENTED_EDGE('',*,*,#6465,.F.);
#8887=ORIENTED_EDGE('',*,*,#6466,.F.);
#8888=ORIENTED_EDGE('',*,*,#6467,.F.);
#8889=ORIENTED_EDGE('',*,*,#6468,.F.);
#8890=ORIENTED_EDGE('',*,*,#6469,.F.);
#8891=ORIENTED_EDGE('',*,*,#6470,.F.);
#8892=ORIENTED_EDGE('',*,*,#6471,.F.);
#8893=ORIENTED_EDGE('',*,*,#6472,.F.);
#8894=ORIENTED_EDGE('',*,*,#6473,.F.);
#8895=ORIENTED_EDGE('',*,*,#6474,.F.);
#8896=ORIENTED_EDGE('',*,*,#6475,.F.);
#8897=ORIENTED_EDGE('',*,*,#6447,.T.);
#8898=ORIENTED_EDGE('',*,*,#6444,.T.);
#8899=ORIENTED_EDGE('',*,*,#6462,.T.);
#8900=ORIENTED_EDGE('',*,*,#6476,.F.);
#8901=ORIENTED_EDGE('',*,*,#6448,.F.);
#8902=ORIENTED_EDGE('',*,*,#6477,.T.);
#8903=ORIENTED_EDGE('',*,*,#6475,.T.);
#8904=ORIENTED_EDGE('',*,*,#6478,.F.);
#8905=ORIENTED_EDGE('',*,*,#6449,.F.);
#8906=ORIENTED_EDGE('',*,*,#6476,.T.);
#8907=ORIENTED_EDGE('',*,*,#6474,.T.);
#8908=ORIENTED_EDGE('',*,*,#6479,.F.);
#8909=ORIENTED_EDGE('',*,*,#6450,.F.);
#8910=ORIENTED_EDGE('',*,*,#6478,.T.);
#8911=ORIENTED_EDGE('',*,*,#6473,.T.);
#8912=ORIENTED_EDGE('',*,*,#6480,.F.);
#8913=ORIENTED_EDGE('',*,*,#6451,.F.);
#8914=ORIENTED_EDGE('',*,*,#6479,.T.);
#8915=ORIENTED_EDGE('',*,*,#6472,.T.);
#8916=ORIENTED_EDGE('',*,*,#6481,.F.);
#8917=ORIENTED_EDGE('',*,*,#6452,.F.);
#8918=ORIENTED_EDGE('',*,*,#6480,.T.);
#8919=ORIENTED_EDGE('',*,*,#6471,.T.);
#8920=ORIENTED_EDGE('',*,*,#6482,.F.);
#8921=ORIENTED_EDGE('',*,*,#6453,.F.);
#8922=ORIENTED_EDGE('',*,*,#6481,.T.);
#8923=ORIENTED_EDGE('',*,*,#6470,.T.);
#8924=ORIENTED_EDGE('',*,*,#6483,.F.);
#8925=ORIENTED_EDGE('',*,*,#6454,.F.);
#8926=ORIENTED_EDGE('',*,*,#6482,.T.);
#8927=ORIENTED_EDGE('',*,*,#6469,.T.);
#8928=ORIENTED_EDGE('',*,*,#6484,.F.);
#8929=ORIENTED_EDGE('',*,*,#6455,.F.);
#8930=ORIENTED_EDGE('',*,*,#6483,.T.);
#8931=ORIENTED_EDGE('',*,*,#6468,.T.);
#8932=ORIENTED_EDGE('',*,*,#6485,.F.);
#8933=ORIENTED_EDGE('',*,*,#6456,.F.);
#8934=ORIENTED_EDGE('',*,*,#6484,.T.);
#8935=ORIENTED_EDGE('',*,*,#6467,.T.);
#8936=ORIENTED_EDGE('',*,*,#6486,.F.);
#8937=ORIENTED_EDGE('',*,*,#6457,.F.);
#8938=ORIENTED_EDGE('',*,*,#6485,.T.);
#8939=ORIENTED_EDGE('',*,*,#6466,.T.);
#8940=ORIENTED_EDGE('',*,*,#6487,.F.);
#8941=ORIENTED_EDGE('',*,*,#6458,.F.);
#8942=ORIENTED_EDGE('',*,*,#6486,.T.);
#8943=ORIENTED_EDGE('',*,*,#6465,.T.);
#8944=ORIENTED_EDGE('',*,*,#6488,.F.);
#8945=ORIENTED_EDGE('',*,*,#6459,.F.);
#8946=ORIENTED_EDGE('',*,*,#6487,.T.);
#8947=ORIENTED_EDGE('',*,*,#6464,.T.);
#8948=ORIENTED_EDGE('',*,*,#6489,.F.);
#8949=ORIENTED_EDGE('',*,*,#6460,.F.);
#8950=ORIENTED_EDGE('',*,*,#6488,.T.);
#8951=ORIENTED_EDGE('',*,*,#6463,.T.);
#8952=ORIENTED_EDGE('',*,*,#6477,.F.);
#8953=ORIENTED_EDGE('',*,*,#6461,.F.);
#8954=ORIENTED_EDGE('',*,*,#6489,.T.);
#8955=ORIENTED_EDGE('',*,*,#6490,.F.);
#8956=ORIENTED_EDGE('',*,*,#6491,.T.);
#8957=ORIENTED_EDGE('',*,*,#6492,.T.);
#8958=ORIENTED_EDGE('',*,*,#6491,.F.);
#8959=ORIENTED_EDGE('',*,*,#6493,.F.);
#8960=ORIENTED_EDGE('',*,*,#6494,.F.);
#8961=ORIENTED_EDGE('',*,*,#6495,.T.);
#8962=ORIENTED_EDGE('',*,*,#6490,.T.);
#8963=ORIENTED_EDGE('',*,*,#6495,.F.);
#8964=ORIENTED_EDGE('',*,*,#6493,.T.);
#8965=ORIENTED_EDGE('',*,*,#6494,.T.);
#8966=ORIENTED_EDGE('',*,*,#6496,.T.);
#8967=ORIENTED_EDGE('',*,*,#6497,.F.);
#8968=ORIENTED_EDGE('',*,*,#6496,.F.);
#8969=ORIENTED_EDGE('',*,*,#6498,.F.);
#8970=ORIENTED_EDGE('',*,*,#6499,.T.);
#8971=ORIENTED_EDGE('',*,*,#6500,.T.);
#8972=ORIENTED_EDGE('',*,*,#6499,.F.);
#8973=ORIENTED_EDGE('',*,*,#6497,.T.);
#8974=ORIENTED_EDGE('',*,*,#6500,.F.);
#8975=ORIENTED_EDGE('',*,*,#6492,.F.);
#8976=ORIENTED_EDGE('',*,*,#6498,.T.);
#8977=ORIENTED_EDGE('',*,*,#6501,.T.);
#8978=ORIENTED_EDGE('',*,*,#6502,.T.);
#8979=ORIENTED_EDGE('',*,*,#6503,.F.);
#8980=ORIENTED_EDGE('',*,*,#6502,.F.);
#8981=ORIENTED_EDGE('',*,*,#6504,.T.);
#8982=ORIENTED_EDGE('',*,*,#6505,.T.);
#8983=ORIENTED_EDGE('',*,*,#6506,.F.);
#8984=ORIENTED_EDGE('',*,*,#6505,.F.);
#8985=ORIENTED_EDGE('',*,*,#6504,.F.);
#8986=ORIENTED_EDGE('',*,*,#6503,.T.);
#8987=ORIENTED_EDGE('',*,*,#6501,.F.);
#8988=ORIENTED_EDGE('',*,*,#6506,.T.);
#8989=ORIENTED_EDGE('',*,*,#6507,.T.);
#8990=ORIENTED_EDGE('',*,*,#6508,.T.);
#8991=ORIENTED_EDGE('',*,*,#6509,.F.);
#8992=ORIENTED_EDGE('',*,*,#6508,.F.);
#8993=ORIENTED_EDGE('',*,*,#6510,.T.);
#8994=ORIENTED_EDGE('',*,*,#6511,.T.);
#8995=ORIENTED_EDGE('',*,*,#6512,.T.);
#8996=ORIENTED_EDGE('',*,*,#6513,.T.);
#8997=ORIENTED_EDGE('',*,*,#6514,.T.);
#8998=ORIENTED_EDGE('',*,*,#6515,.T.);
#8999=ORIENTED_EDGE('',*,*,#6507,.F.);
#9000=ORIENTED_EDGE('',*,*,#6516,.F.);
#9001=ORIENTED_EDGE('',*,*,#6517,.F.);
#9002=ORIENTED_EDGE('',*,*,#6518,.F.);
#9003=ORIENTED_EDGE('',*,*,#6519,.F.);
#9004=ORIENTED_EDGE('',*,*,#6520,.F.);
#9005=ORIENTED_EDGE('',*,*,#6521,.F.);
#9006=ORIENTED_EDGE('',*,*,#6509,.T.);
#9007=ORIENTED_EDGE('',*,*,#6516,.T.);
#9008=ORIENTED_EDGE('',*,*,#6522,.F.);
#9009=ORIENTED_EDGE('',*,*,#6510,.F.);
#9010=ORIENTED_EDGE('',*,*,#6523,.T.);
#9011=ORIENTED_EDGE('',*,*,#6521,.T.);
#9012=ORIENTED_EDGE('',*,*,#6524,.F.);
#9013=ORIENTED_EDGE('',*,*,#6511,.F.);
#9014=ORIENTED_EDGE('',*,*,#6522,.T.);
#9015=ORIENTED_EDGE('',*,*,#6520,.T.);
#9016=ORIENTED_EDGE('',*,*,#6525,.F.);
#9017=ORIENTED_EDGE('',*,*,#6512,.F.);
#9018=ORIENTED_EDGE('',*,*,#6524,.T.);
#9019=ORIENTED_EDGE('',*,*,#6519,.T.);
#9020=ORIENTED_EDGE('',*,*,#6526,.F.);
#9021=ORIENTED_EDGE('',*,*,#6513,.F.);
#9022=ORIENTED_EDGE('',*,*,#6525,.T.);
#9023=ORIENTED_EDGE('',*,*,#6518,.T.);
#9024=ORIENTED_EDGE('',*,*,#6527,.F.);
#9025=ORIENTED_EDGE('',*,*,#6514,.F.);
#9026=ORIENTED_EDGE('',*,*,#6526,.T.);
#9027=ORIENTED_EDGE('',*,*,#6517,.T.);
#9028=ORIENTED_EDGE('',*,*,#6523,.F.);
#9029=ORIENTED_EDGE('',*,*,#6515,.F.);
#9030=ORIENTED_EDGE('',*,*,#6527,.T.);
#9031=ORIENTED_EDGE('',*,*,#6528,.T.);
#9032=ORIENTED_EDGE('',*,*,#6529,.T.);
#9033=ORIENTED_EDGE('',*,*,#6530,.F.);
#9034=ORIENTED_EDGE('',*,*,#6529,.F.);
#9035=ORIENTED_EDGE('',*,*,#6531,.T.);
#9036=ORIENTED_EDGE('',*,*,#6532,.T.);
#9037=ORIENTED_EDGE('',*,*,#6533,.F.);
#9038=ORIENTED_EDGE('',*,*,#6532,.F.);
#9039=ORIENTED_EDGE('',*,*,#6531,.F.);
#9040=ORIENTED_EDGE('',*,*,#6534,.F.);
#9041=ORIENTED_EDGE('',*,*,#6535,.F.);
#9042=ORIENTED_EDGE('',*,*,#6536,.F.);
#9043=ORIENTED_EDGE('',*,*,#6537,.F.);
#9044=ORIENTED_EDGE('',*,*,#6538,.F.);
#9045=ORIENTED_EDGE('',*,*,#6539,.F.);
#9046=ORIENTED_EDGE('',*,*,#6533,.T.);
#9047=ORIENTED_EDGE('',*,*,#6528,.F.);
#9048=ORIENTED_EDGE('',*,*,#6530,.T.);
#9049=ORIENTED_EDGE('',*,*,#6534,.T.);
#9050=ORIENTED_EDGE('',*,*,#6540,.F.);
#9051=ORIENTED_EDGE('',*,*,#6541,.T.);
#9052=ORIENTED_EDGE('',*,*,#6542,.T.);
#9053=ORIENTED_EDGE('',*,*,#6535,.T.);
#9054=ORIENTED_EDGE('',*,*,#6542,.F.);
#9055=ORIENTED_EDGE('',*,*,#6543,.T.);
#9056=ORIENTED_EDGE('',*,*,#6544,.T.);
#9057=ORIENTED_EDGE('',*,*,#6536,.T.);
#9058=ORIENTED_EDGE('',*,*,#6544,.F.);
#9059=ORIENTED_EDGE('',*,*,#6545,.T.);
#9060=ORIENTED_EDGE('',*,*,#6546,.T.);
#9061=ORIENTED_EDGE('',*,*,#6537,.T.);
#9062=ORIENTED_EDGE('',*,*,#6546,.F.);
#9063=ORIENTED_EDGE('',*,*,#6547,.T.);
#9064=ORIENTED_EDGE('',*,*,#6548,.T.);
#9065=ORIENTED_EDGE('',*,*,#6538,.T.);
#9066=ORIENTED_EDGE('',*,*,#6548,.F.);
#9067=ORIENTED_EDGE('',*,*,#6549,.T.);
#9068=ORIENTED_EDGE('',*,*,#6550,.T.);
#9069=ORIENTED_EDGE('',*,*,#6539,.T.);
#9070=ORIENTED_EDGE('',*,*,#6550,.F.);
#9071=ORIENTED_EDGE('',*,*,#6551,.T.);
#9072=ORIENTED_EDGE('',*,*,#6540,.T.);
#9073=ORIENTED_EDGE('',*,*,#6541,.F.);
#9074=ORIENTED_EDGE('',*,*,#6551,.F.);
#9075=ORIENTED_EDGE('',*,*,#6549,.F.);
#9076=ORIENTED_EDGE('',*,*,#6547,.F.);
#9077=ORIENTED_EDGE('',*,*,#6545,.F.);
#9078=ORIENTED_EDGE('',*,*,#6543,.F.);
#9079=ORIENTED_EDGE('',*,*,#6552,.T.);
#9080=ORIENTED_EDGE('',*,*,#6553,.T.);
#9081=ORIENTED_EDGE('',*,*,#6554,.F.);
#9082=ORIENTED_EDGE('',*,*,#6553,.F.);
#9083=ORIENTED_EDGE('',*,*,#6555,.T.);
#9084=ORIENTED_EDGE('',*,*,#6556,.F.);
#9085=ORIENTED_EDGE('',*,*,#6557,.F.);
#9086=ORIENTED_EDGE('',*,*,#6558,.T.);
#9087=ORIENTED_EDGE('',*,*,#6559,.T.);
#9088=ORIENTED_EDGE('',*,*,#6560,.F.);
#9089=ORIENTED_EDGE('',*,*,#6561,.F.);
#9090=ORIENTED_EDGE('',*,*,#6556,.T.);
#9091=ORIENTED_EDGE('',*,*,#6562,.T.);
#9092=ORIENTED_EDGE('',*,*,#6563,.F.);
#9093=ORIENTED_EDGE('',*,*,#6564,.F.);
#9094=ORIENTED_EDGE('',*,*,#6560,.T.);
#9095=ORIENTED_EDGE('',*,*,#6565,.T.);
#9096=ORIENTED_EDGE('',*,*,#6566,.F.);
#9097=ORIENTED_EDGE('',*,*,#6567,.F.);
#9098=ORIENTED_EDGE('',*,*,#6563,.T.);
#9099=ORIENTED_EDGE('',*,*,#6568,.T.);
#9100=ORIENTED_EDGE('',*,*,#6569,.F.);
#9101=ORIENTED_EDGE('',*,*,#6570,.F.);
#9102=ORIENTED_EDGE('',*,*,#6566,.T.);
#9103=ORIENTED_EDGE('',*,*,#6571,.T.);
#9104=ORIENTED_EDGE('',*,*,#6558,.F.);
#9105=ORIENTED_EDGE('',*,*,#6572,.F.);
#9106=ORIENTED_EDGE('',*,*,#6569,.T.);
#9107=ORIENTED_EDGE('',*,*,#6557,.T.);
#9108=ORIENTED_EDGE('',*,*,#6561,.T.);
#9109=ORIENTED_EDGE('',*,*,#6564,.T.);
#9110=ORIENTED_EDGE('',*,*,#6567,.T.);
#9111=ORIENTED_EDGE('',*,*,#6570,.T.);
#9112=ORIENTED_EDGE('',*,*,#6572,.T.);
#9113=ORIENTED_EDGE('',*,*,#6552,.F.);
#9114=ORIENTED_EDGE('',*,*,#6555,.F.);
#9115=ORIENTED_EDGE('',*,*,#6571,.F.);
#9116=ORIENTED_EDGE('',*,*,#6568,.F.);
#9117=ORIENTED_EDGE('',*,*,#6565,.F.);
#9118=ORIENTED_EDGE('',*,*,#6562,.F.);
#9119=ORIENTED_EDGE('',*,*,#6559,.F.);
#9120=ORIENTED_EDGE('',*,*,#6554,.T.);
#9121=ORIENTED_EDGE('',*,*,#6573,.T.);
#9122=ORIENTED_EDGE('',*,*,#6574,.T.);
#9123=ORIENTED_EDGE('',*,*,#6575,.F.);
#9124=ORIENTED_EDGE('',*,*,#6574,.F.);
#9125=ORIENTED_EDGE('',*,*,#6576,.T.);
#9126=ORIENTED_EDGE('',*,*,#6577,.T.);
#9127=ORIENTED_EDGE('',*,*,#6578,.F.);
#9128=ORIENTED_EDGE('',*,*,#6577,.F.);
#9129=ORIENTED_EDGE('',*,*,#6576,.F.);
#9130=ORIENTED_EDGE('',*,*,#6579,.F.);
#9131=ORIENTED_EDGE('',*,*,#6580,.F.);
#9132=ORIENTED_EDGE('',*,*,#6581,.F.);
#9133=ORIENTED_EDGE('',*,*,#6582,.F.);
#9134=ORIENTED_EDGE('',*,*,#6583,.F.);
#9135=ORIENTED_EDGE('',*,*,#6584,.F.);
#9136=ORIENTED_EDGE('',*,*,#6578,.T.);
#9137=ORIENTED_EDGE('',*,*,#6573,.F.);
#9138=ORIENTED_EDGE('',*,*,#6575,.T.);
#9139=ORIENTED_EDGE('',*,*,#6579,.T.);
#9140=ORIENTED_EDGE('',*,*,#6585,.F.);
#9141=ORIENTED_EDGE('',*,*,#6586,.T.);
#9142=ORIENTED_EDGE('',*,*,#6587,.T.);
#9143=ORIENTED_EDGE('',*,*,#6580,.T.);
#9144=ORIENTED_EDGE('',*,*,#6587,.F.);
#9145=ORIENTED_EDGE('',*,*,#6588,.T.);
#9146=ORIENTED_EDGE('',*,*,#6589,.T.);
#9147=ORIENTED_EDGE('',*,*,#6581,.T.);
#9148=ORIENTED_EDGE('',*,*,#6589,.F.);
#9149=ORIENTED_EDGE('',*,*,#6590,.T.);
#9150=ORIENTED_EDGE('',*,*,#6591,.T.);
#9151=ORIENTED_EDGE('',*,*,#6582,.T.);
#9152=ORIENTED_EDGE('',*,*,#6591,.F.);
#9153=ORIENTED_EDGE('',*,*,#6592,.T.);
#9154=ORIENTED_EDGE('',*,*,#6593,.T.);
#9155=ORIENTED_EDGE('',*,*,#6583,.T.);
#9156=ORIENTED_EDGE('',*,*,#6593,.F.);
#9157=ORIENTED_EDGE('',*,*,#6594,.T.);
#9158=ORIENTED_EDGE('',*,*,#6595,.T.);
#9159=ORIENTED_EDGE('',*,*,#6584,.T.);
#9160=ORIENTED_EDGE('',*,*,#6595,.F.);
#9161=ORIENTED_EDGE('',*,*,#6596,.T.);
#9162=ORIENTED_EDGE('',*,*,#6585,.T.);
#9163=ORIENTED_EDGE('',*,*,#6586,.F.);
#9164=ORIENTED_EDGE('',*,*,#6596,.F.);
#9165=ORIENTED_EDGE('',*,*,#6594,.F.);
#9166=ORIENTED_EDGE('',*,*,#6592,.F.);
#9167=ORIENTED_EDGE('',*,*,#6590,.F.);
#9168=ORIENTED_EDGE('',*,*,#6588,.F.);
#9169=CYLINDRICAL_SURFACE('',#10078,2.5);
#9170=CYLINDRICAL_SURFACE('',#10081,2.5);
#9171=CYLINDRICAL_SURFACE('',#10131,14.2);
#9172=CYLINDRICAL_SURFACE('',#10133,14.2);
#9173=CYLINDRICAL_SURFACE('',#10136,2.5);
#9174=CYLINDRICAL_SURFACE('',#10139,2.5);
#9175=CYLINDRICAL_SURFACE('',#10142,2.6);
#9176=CYLINDRICAL_SURFACE('',#10147,2.6);
#9177=CYLINDRICAL_SURFACE('',#10152,2.6);
#9178=CYLINDRICAL_SURFACE('',#10190,2.59999999999999);
#9179=CYLINDRICAL_SURFACE('',#10195,2.59999999999999);
#9180=CYLINDRICAL_SURFACE('',#10200,2.59999999999999);
#9181=CYLINDRICAL_SURFACE('',#10205,2.5);
#9182=CYLINDRICAL_SURFACE('',#10208,2.5);
#9183=CYLINDRICAL_SURFACE('',#10211,9.1);
#9184=CYLINDRICAL_SURFACE('',#10267,1.65);
#9185=CYLINDRICAL_SURFACE('',#10270,1.65);
#9186=CYLINDRICAL_SURFACE('',#10273,2.5);
#9187=CYLINDRICAL_SURFACE('',#10276,2.5);
#9188=CYLINDRICAL_SURFACE('',#10279,6.15);
#9189=CYLINDRICAL_SURFACE('',#10314,3.7);
#9190=CYLINDRICAL_SURFACE('',#10317,3.7);
#9191=CYLINDRICAL_SURFACE('',#10320,2.2);
#9192=CYLINDRICAL_SURFACE('',#10323,2.2);
#9193=CYLINDRICAL_SURFACE('',#10335,5.55);
#9194=CYLINDRICAL_SURFACE('',#10338,6.);
#9195=CYLINDRICAL_SURFACE('',#10341,9.);
#9196=CYLINDRICAL_SURFACE('',#10344,6.);
#9197=CYLINDRICAL_SURFACE('',#10347,4.);
#9198=CYLINDRICAL_SURFACE('',#10357,7.15);
#9199=CYLINDRICAL_SURFACE('',#10360,6.);
#9200=CYLINDRICAL_SURFACE('',#10363,9.);
#9201=CYLINDRICAL_SURFACE('',#10366,6.);
#9202=CYLINDRICAL_SURFACE('',#10369,4.);
#9203=CYLINDRICAL_SURFACE('',#10379,2.2);
#9204=CYLINDRICAL_SURFACE('',#10381,2.2);
#9205=CYLINDRICAL_SURFACE('',#10383,6.);
#9206=CYLINDRICAL_SURFACE('',#10386,8.75);
#9207=CYLINDRICAL_SURFACE('',#10389,10.);
#9208=CYLINDRICAL_SURFACE('',#10405,5.75);
#9209=CYLINDRICAL_SURFACE('',#10415,7.35);
#9210=CYLINDRICAL_SURFACE('',#10425,2.19999999999999);
#9211=CYLINDRICAL_SURFACE('',#10428,7.00000000000001);
#9212=CYLINDRICAL_SURFACE('',#10431,5.);
#9213=CYLINDRICAL_SURFACE('',#10434,3.);
#9214=CYLINDRICAL_SURFACE('',#10441,2.);
#9215=CYLINDRICAL_SURFACE('',#10447,5.50000000000001);
#9216=CYLINDRICAL_SURFACE('',#10450,5.50000000000001);
#9217=CYLINDRICAL_SURFACE('',#10453,3.3);
#9218=CYLINDRICAL_SURFACE('',#10456,3.3);
#9219=CYLINDRICAL_SURFACE('',#10468,3.3);
#9220=CYLINDRICAL_SURFACE('',#10471,3.3);
#9221=CYLINDRICAL_SURFACE('',#10474,6.2);
#9222=CYLINDRICAL_SURFACE('',#10488,6.2);
#9223=CYLINDRICAL_SURFACE('',#10491,14.);
#9224=CYLINDRICAL_SURFACE('',#10779,3.2);
#9225=CYLINDRICAL_SURFACE('',#10782,4.2);
#9226=CYLINDRICAL_SURFACE('',#10805,9.);
#9227=CYLINDRICAL_SURFACE('',#10810,3.2);
#9228=CYLINDRICAL_SURFACE('',#10816,5.);
#9229=CYLINDRICAL_SURFACE('',#10819,3.);
#9230=CYLINDRICAL_SURFACE('',#10826,4.2);
#9231=CYLINDRICAL_SURFACE('',#10838,2.4);
#9232=CYLINDRICAL_SURFACE('',#10841,5.);
#9233=CYLINDRICAL_SURFACE('',#10855,2.);
#9234=CYLINDRICAL_SURFACE('',#10868,1.5);
#9235=CYLINDRICAL_SURFACE('',#10871,3.5);
#9236=ADVANCED_FACE('',(#911),#9169,.F.);
#9237=ADVANCED_FACE('',(#912),#9170,.F.);
#9238=ADVANCED_FACE('',(#913,#306,#307),#429,.F.);
#9239=ADVANCED_FACE('',(#914),#430,.F.);
#9240=ADVANCED_FACE('',(#915),#431,.F.);
#9241=ADVANCED_FACE('',(#916),#432,.F.);
#9242=ADVANCED_FACE('',(#917),#433,.F.);
#9243=ADVANCED_FACE('',(#918),#434,.F.);
#9244=ADVANCED_FACE('',(#919),#435,.F.);
#9245=ADVANCED_FACE('',(#920),#436,.F.);
#9246=ADVANCED_FACE('',(#921),#437,.F.);
#9247=ADVANCED_FACE('',(#922),#438,.T.);
#9248=ADVANCED_FACE('',(#923),#439,.F.);
#9249=ADVANCED_FACE('',(#924),#440,.F.);
#9250=ADVANCED_FACE('',(#925),#441,.F.);
#9251=ADVANCED_FACE('',(#926),#442,.F.);
#9252=ADVANCED_FACE('',(#927),#443,.F.);
#9253=ADVANCED_FACE('',(#928),#444,.F.);
#9254=ADVANCED_FACE('',(#929),#445,.T.);
#9255=ADVANCED_FACE('',(#930,#308),#446,.F.);
#9256=ADVANCED_FACE('',(#931),#447,.F.);
#9257=ADVANCED_FACE('',(#932),#448,.F.);
#9258=ADVANCED_FACE('',(#933),#449,.F.);
#9259=ADVANCED_FACE('',(#934),#450,.F.);
#9260=ADVANCED_FACE('',(#935),#451,.F.);
#9261=ADVANCED_FACE('',(#936,#309),#452,.T.);
#9262=ADVANCED_FACE('',(#937),#453,.T.);
#9263=ADVANCED_FACE('',(#938),#454,.T.);
#9264=ADVANCED_FACE('',(#939),#455,.T.);
#9265=ADVANCED_FACE('',(#940),#456,.T.);
#9266=ADVANCED_FACE('',(#941),#457,.T.);
#9267=ADVANCED_FACE('',(#942),#458,.T.);
#9268=ADVANCED_FACE('',(#943),#459,.T.);
#9269=ADVANCED_FACE('',(#944),#460,.T.);
#9270=ADVANCED_FACE('',(#945),#461,.T.);
#9271=ADVANCED_FACE('',(#946),#462,.T.);
#9272=ADVANCED_FACE('',(#947),#463,.T.);
#9273=ADVANCED_FACE('',(#948),#464,.T.);
#9274=ADVANCED_FACE('',(#949),#465,.T.);
#9275=ADVANCED_FACE('',(#950),#466,.T.);
#9276=ADVANCED_FACE('',(#951),#467,.T.);
#9277=ADVANCED_FACE('',(#952),#468,.T.);
#9278=ADVANCED_FACE('',(#953),#469,.T.);
#9279=ADVANCED_FACE('',(#954),#470,.T.);
#9280=ADVANCED_FACE('',(#955),#471,.F.);
#9281=ADVANCED_FACE('',(#956),#472,.F.);
#9282=ADVANCED_FACE('',(#957),#473,.F.);
#9283=ADVANCED_FACE('',(#958),#9171,.F.);
#9284=ADVANCED_FACE('',(#959),#9172,.F.);
#9285=ADVANCED_FACE('',(#960),#9173,.F.);
#9286=ADVANCED_FACE('',(#961),#9174,.F.);
#9287=ADVANCED_FACE('',(#962),#9175,.F.);
#9288=ADVANCED_FACE('',(#963),#9176,.F.);
#9289=ADVANCED_FACE('',(#964),#9177,.F.);
#9290=ADVANCED_FACE('',(#965,#310,#311),#474,.F.);
#9291=ADVANCED_FACE('',(#966,#312,#313,#314),#475,.F.);
#9292=ADVANCED_FACE('',(#967),#476,.F.);
#9293=ADVANCED_FACE('',(#968),#477,.F.);
#9294=ADVANCED_FACE('',(#969),#478,.F.);
#9295=ADVANCED_FACE('',(#970),#479,.F.);
#9296=ADVANCED_FACE('',(#971),#480,.F.);
#9297=ADVANCED_FACE('',(#972),#481,.F.);
#9298=ADVANCED_FACE('',(#973),#482,.F.);
#9299=ADVANCED_FACE('',(#974,#315,#316,#317),#483,.F.);
#9300=ADVANCED_FACE('',(#975),#484,.F.);
#9301=ADVANCED_FACE('',(#976),#485,.F.);
#9302=ADVANCED_FACE('',(#977),#486,.T.);
#9303=ADVANCED_FACE('',(#978),#487,.F.);
#9304=ADVANCED_FACE('',(#979),#488,.F.);
#9305=ADVANCED_FACE('',(#980),#489,.F.);
#9306=ADVANCED_FACE('',(#981),#490,.F.);
#9307=ADVANCED_FACE('',(#982),#491,.F.);
#9308=ADVANCED_FACE('',(#983,#318),#492,.F.);
#9309=ADVANCED_FACE('',(#984),#493,.T.);
#9310=ADVANCED_FACE('',(#985),#494,.F.);
#9311=ADVANCED_FACE('',(#986),#495,.F.);
#9312=ADVANCED_FACE('',(#987),#496,.F.);
#9313=ADVANCED_FACE('',(#988),#497,.F.);
#9314=ADVANCED_FACE('',(#989,#319),#498,.T.);
#9315=ADVANCED_FACE('',(#990),#499,.F.);
#9316=ADVANCED_FACE('',(#991),#500,.T.);
#9317=ADVANCED_FACE('',(#992),#501,.T.);
#9318=ADVANCED_FACE('',(#993),#502,.T.);
#9319=ADVANCED_FACE('',(#994),#503,.T.);
#9320=ADVANCED_FACE('',(#995),#504,.T.);
#9321=ADVANCED_FACE('',(#996),#505,.T.);
#9322=ADVANCED_FACE('',(#997),#9178,.F.);
#9323=ADVANCED_FACE('',(#998),#9179,.F.);
#9324=ADVANCED_FACE('',(#999),#9180,.F.);
#9325=ADVANCED_FACE('',(#1000),#9181,.F.);
#9326=ADVANCED_FACE('',(#1001),#9182,.F.);
#9327=ADVANCED_FACE('',(#1002),#9183,.F.);
#9328=ADVANCED_FACE('',(#1003,#320),#506,.F.);
#9329=ADVANCED_FACE('',(#1004),#507,.T.);
#9330=ADVANCED_FACE('',(#1005),#508,.T.);
#9331=ADVANCED_FACE('',(#1006),#509,.T.);
#9332=ADVANCED_FACE('',(#1007),#510,.T.);
#9333=ADVANCED_FACE('',(#1008),#511,.T.);
#9334=ADVANCED_FACE('',(#1009),#512,.T.);
#9335=ADVANCED_FACE('',(#1010),#513,.T.);
#9336=ADVANCED_FACE('',(#1011),#514,.T.);
#9337=ADVANCED_FACE('',(#1012),#515,.T.);
#9338=ADVANCED_FACE('',(#1013),#516,.T.);
#9339=ADVANCED_FACE('',(#1014),#517,.T.);
#9340=ADVANCED_FACE('',(#1015),#518,.T.);
#9341=ADVANCED_FACE('',(#1016,#321,#322,#323),#519,.F.);
#9342=ADVANCED_FACE('',(#1017,#324,#325,#326),#520,.F.);
#9343=ADVANCED_FACE('',(#1018),#521,.F.);
#9344=ADVANCED_FACE('',(#1019),#522,.F.);
#9345=ADVANCED_FACE('',(#1020),#523,.F.);
#9346=ADVANCED_FACE('',(#1021),#524,.F.);
#9347=ADVANCED_FACE('',(#1022),#525,.F.);
#9348=ADVANCED_FACE('',(#1023),#526,.F.);
#9349=ADVANCED_FACE('',(#1024,#327),#527,.F.);
#9350=ADVANCED_FACE('',(#1025),#528,.T.);
#9351=ADVANCED_FACE('',(#1026),#529,.F.);
#9352=ADVANCED_FACE('',(#1027),#530,.F.);
#9353=ADVANCED_FACE('',(#1028),#531,.F.);
#9354=ADVANCED_FACE('',(#1029),#532,.F.);
#9355=ADVANCED_FACE('',(#1030),#533,.F.);
#9356=ADVANCED_FACE('',(#1031),#534,.F.);
#9357=ADVANCED_FACE('',(#1032,#328,#329),#535,.T.);
#9358=ADVANCED_FACE('',(#1033),#536,.F.);
#9359=ADVANCED_FACE('',(#1034),#537,.F.);
#9360=ADVANCED_FACE('',(#1035),#538,.F.);
#9361=ADVANCED_FACE('',(#1036),#539,.F.);
#9362=ADVANCED_FACE('',(#1037),#540,.F.);
#9363=ADVANCED_FACE('',(#1038,#330),#541,.F.);
#9364=ADVANCED_FACE('',(#1039),#542,.T.);
#9365=ADVANCED_FACE('',(#1040),#543,.F.);
#9366=ADVANCED_FACE('',(#1041),#544,.T.);
#9367=ADVANCED_FACE('',(#1042),#545,.T.);
#9368=ADVANCED_FACE('',(#1043),#546,.F.);
#9369=ADVANCED_FACE('',(#1044),#547,.F.);
#9370=ADVANCED_FACE('',(#1045),#548,.T.);
#9371=ADVANCED_FACE('',(#1046),#549,.T.);
#9372=ADVANCED_FACE('',(#1047),#550,.T.);
#9373=ADVANCED_FACE('',(#1048),#551,.T.);
#9374=ADVANCED_FACE('',(#1049),#552,.T.);
#9375=ADVANCED_FACE('',(#1050),#553,.T.);
#9376=ADVANCED_FACE('',(#1051),#554,.T.);
#9377=ADVANCED_FACE('',(#1052),#555,.T.);
#9378=ADVANCED_FACE('',(#1053),#556,.T.);
#9379=ADVANCED_FACE('',(#1054),#557,.T.);
#9380=ADVANCED_FACE('',(#1055),#9184,.F.);
#9381=ADVANCED_FACE('',(#1056),#9185,.F.);
#9382=ADVANCED_FACE('',(#1057),#9186,.F.);
#9383=ADVANCED_FACE('',(#1058),#9187,.F.);
#9384=ADVANCED_FACE('',(#1059),#9188,.F.);
#9385=ADVANCED_FACE('',(#1060),#558,.F.);
#9386=ADVANCED_FACE('',(#1061),#559,.F.);
#9387=ADVANCED_FACE('',(#1062),#560,.F.);
#9388=ADVANCED_FACE('',(#1063),#561,.F.);
#9389=ADVANCED_FACE('',(#1064),#562,.F.);
#9390=ADVANCED_FACE('',(#1065),#563,.F.);
#9391=ADVANCED_FACE('',(#1066),#564,.F.);
#9392=ADVANCED_FACE('',(#1067,#331,#332),#565,.F.);
#9393=ADVANCED_FACE('',(#1068,#333),#566,.T.);
#9394=ADVANCED_FACE('',(#1069),#567,.F.);
#9395=ADVANCED_FACE('',(#1070),#568,.F.);
#9396=ADVANCED_FACE('',(#1071,#334,#335),#569,.T.);
#9397=ADVANCED_FACE('',(#1072),#570,.F.);
#9398=ADVANCED_FACE('',(#1073),#571,.T.);
#9399=ADVANCED_FACE('',(#1074),#572,.T.);
#9400=ADVANCED_FACE('',(#1075),#573,.F.);
#9401=ADVANCED_FACE('',(#1076),#574,.F.);
#9402=ADVANCED_FACE('',(#1077),#575,.F.);
#9403=ADVANCED_FACE('',(#1078),#576,.F.);
#9404=ADVANCED_FACE('',(#1079),#577,.F.);
#9405=ADVANCED_FACE('',(#1080),#578,.F.);
#9406=ADVANCED_FACE('',(#1081),#579,.T.);
#9407=ADVANCED_FACE('',(#1082),#580,.F.);
#9408=ADVANCED_FACE('',(#1083),#581,.F.);
#9409=ADVANCED_FACE('',(#1084),#582,.F.);
#9410=ADVANCED_FACE('',(#1085),#583,.F.);
#9411=ADVANCED_FACE('',(#1086),#584,.F.);
#9412=ADVANCED_FACE('',(#1087),#585,.F.);
#9413=ADVANCED_FACE('',(#1088),#586,.T.);
#9414=ADVANCED_FACE('',(#1089),#9189,.F.);
#9415=ADVANCED_FACE('',(#1090),#9190,.F.);
#9416=ADVANCED_FACE('',(#1091),#9191,.F.);
#9417=ADVANCED_FACE('',(#1092),#9192,.F.);
#9418=ADVANCED_FACE('',(#1093),#587,.F.);
#9419=ADVANCED_FACE('',(#1094),#588,.F.);
#9420=ADVANCED_FACE('',(#1095),#589,.F.);
#9421=ADVANCED_FACE('',(#1096),#590,.F.);
#9422=ADVANCED_FACE('',(#1097,#336,#337),#591,.F.);
#9423=ADVANCED_FACE('',(#1098,#338,#339),#592,.T.);
#9424=ADVANCED_FACE('',(#1099,#340),#593,.F.);
#9425=ADVANCED_FACE('',(#1100,#341),#594,.F.);
#9426=ADVANCED_FACE('',(#1101),#9193,.T.);
#9427=ADVANCED_FACE('',(#1102),#9194,.T.);
#9428=ADVANCED_FACE('',(#1103),#9195,.T.);
#9429=ADVANCED_FACE('',(#1104),#9196,.T.);
#9430=ADVANCED_FACE('',(#1105),#9197,.T.);
#9431=ADVANCED_FACE('',(#1106),#595,.F.);
#9432=ADVANCED_FACE('',(#1107,#342),#596,.F.);
#9433=ADVANCED_FACE('',(#1108,#343),#597,.F.);
#9434=ADVANCED_FACE('',(#1109,#344),#598,.F.);
#9435=ADVANCED_FACE('',(#1110,#345),#599,.F.);
#9436=ADVANCED_FACE('',(#1111),#600,.F.);
#9437=ADVANCED_FACE('',(#1112),#9198,.T.);
#9438=ADVANCED_FACE('',(#1113),#9199,.T.);
#9439=ADVANCED_FACE('',(#1114),#9200,.T.);
#9440=ADVANCED_FACE('',(#1115),#9201,.T.);
#9441=ADVANCED_FACE('',(#1116),#9202,.T.);
#9442=ADVANCED_FACE('',(#1117),#601,.F.);
#9443=ADVANCED_FACE('',(#1118,#346),#602,.F.);
#9444=ADVANCED_FACE('',(#1119,#347),#603,.F.);
#9445=ADVANCED_FACE('',(#1120,#348),#604,.F.);
#9446=ADVANCED_FACE('',(#1121,#349),#605,.F.);
#9447=ADVANCED_FACE('',(#1122),#606,.F.);
#9448=ADVANCED_FACE('',(#1123),#9203,.F.);
#9449=ADVANCED_FACE('',(#1124),#9204,.F.);
#9450=ADVANCED_FACE('',(#1125),#9205,.T.);
#9451=ADVANCED_FACE('',(#1126),#9206,.T.);
#9452=ADVANCED_FACE('',(#1127,#350),#9207,.T.);
#9453=ADVANCED_FACE('',(#1128),#607,.F.);
#9454=ADVANCED_FACE('',(#1129),#608,.F.);
#9455=ADVANCED_FACE('',(#1130,#351),#609,.F.);
#9456=ADVANCED_FACE('',(#1131,#352),#610,.F.);
#9457=ADVANCED_FACE('',(#1132),#611,.F.);
#9458=ADVANCED_FACE('',(#1133,#353),#612,.T.);
#9459=ADVANCED_FACE('',(#1134,#354),#613,.T.);
#9460=ADVANCED_FACE('',(#1135),#614,.F.);
#9461=ADVANCED_FACE('',(#1136),#9208,.F.);
#9462=ADVANCED_FACE('',(#1137,#355),#615,.T.);
#9463=ADVANCED_FACE('',(#1138,#356),#616,.F.);
#9464=ADVANCED_FACE('',(#1139),#617,.F.);
#9465=ADVANCED_FACE('',(#1140),#618,.F.);
#9466=ADVANCED_FACE('',(#1141),#619,.F.);
#9467=ADVANCED_FACE('',(#1142),#620,.F.);
#9468=ADVANCED_FACE('',(#1143),#9209,.F.);
#9469=ADVANCED_FACE('',(#1144,#357),#621,.T.);
#9470=ADVANCED_FACE('',(#1145,#358),#622,.F.);
#9471=ADVANCED_FACE('',(#1146),#623,.F.);
#9472=ADVANCED_FACE('',(#1147),#624,.F.);
#9473=ADVANCED_FACE('',(#1148),#625,.F.);
#9474=ADVANCED_FACE('',(#1149),#626,.F.);
#9475=ADVANCED_FACE('',(#1150),#9210,.F.);
#9476=ADVANCED_FACE('',(#1151),#9211,.T.);
#9477=ADVANCED_FACE('',(#1152),#9212,.T.);
#9478=ADVANCED_FACE('',(#1153),#9213,.T.);
#9479=ADVANCED_FACE('',(#1154,#359),#627,.T.);
#9480=ADVANCED_FACE('',(#1155),#628,.F.);
#9481=ADVANCED_FACE('',(#1156,#360),#629,.T.);
#9482=ADVANCED_FACE('',(#1157,#361),#630,.F.);
#9483=ADVANCED_FACE('',(#1158),#9214,.T.);
#9484=ADVANCED_FACE('',(#1159),#631,.T.);
#9485=ADVANCED_FACE('',(#1160),#632,.F.);
#9486=ADVANCED_FACE('',(#1161),#9215,.F.);
#9487=ADVANCED_FACE('',(#1162),#9216,.F.);
#9488=ADVANCED_FACE('',(#1163),#9217,.F.);
#9489=ADVANCED_FACE('',(#1164),#9218,.F.);
#9490=ADVANCED_FACE('',(#1165),#633,.F.);
#9491=ADVANCED_FACE('',(#1166),#634,.F.);
#9492=ADVANCED_FACE('',(#1167),#635,.F.);
#9493=ADVANCED_FACE('',(#1168),#636,.F.);
#9494=ADVANCED_FACE('',(#1169,#362,#363),#637,.T.);
#9495=ADVANCED_FACE('',(#1170,#364,#365),#638,.F.);
#9496=ADVANCED_FACE('',(#1171,#366),#639,.F.);
#9497=ADVANCED_FACE('',(#1172,#367),#640,.F.);
#9498=ADVANCED_FACE('',(#1173),#9219,.F.);
#9499=ADVANCED_FACE('',(#1174),#9220,.F.);
#9500=ADVANCED_FACE('',(#1175),#9221,.F.);
#9501=ADVANCED_FACE('',(#1176,#368,#369,#370),#641,.T.);
#9502=ADVANCED_FACE('',(#1177,#371,#372,#373),#642,.F.);
#9503=ADVANCED_FACE('',(#1178),#643,.F.);
#9504=ADVANCED_FACE('',(#1179),#644,.F.);
#9505=ADVANCED_FACE('',(#1180),#645,.F.);
#9506=ADVANCED_FACE('',(#1181),#646,.F.);
#9507=ADVANCED_FACE('',(#1182),#647,.F.);
#9508=ADVANCED_FACE('',(#1183),#648,.F.);
#9509=ADVANCED_FACE('',(#1184),#649,.F.);
#9510=ADVANCED_FACE('',(#1185),#650,.F.);
#9511=ADVANCED_FACE('',(#1186),#9222,.F.);
#9512=ADVANCED_FACE('',(#1187,#374,#375,#376,#377,#378,#379,#380,#381,#382,
#383,#384,#385,#386,#387,#388,#389,#390,#391,#392,#393,#394,#395,#396,#397,
#398,#399,#400,#401,#402,#403,#404,#405,#406,#407,#408,#409,#410,#411,#412),
#9223,.T.);
#9513=ADVANCED_FACE('',(#1188,#413),#651,.T.);
#9514=ADVANCED_FACE('',(#1189,#414),#652,.F.);
#9515=ADVANCED_FACE('',(#1190),#653,.T.);
#9516=ADVANCED_FACE('',(#1191),#654,.T.);
#9517=ADVANCED_FACE('',(#1192),#655,.F.);
#9518=ADVANCED_FACE('',(#1193),#656,.T.);
#9519=ADVANCED_FACE('',(#1194),#657,.T.);
#9520=ADVANCED_FACE('',(#1195),#658,.T.);
#9521=ADVANCED_FACE('',(#1196),#659,.T.);
#9522=ADVANCED_FACE('',(#1197),#660,.F.);
#9523=ADVANCED_FACE('',(#1198),#661,.T.);
#9524=ADVANCED_FACE('',(#1199),#662,.T.);
#9525=ADVANCED_FACE('',(#1200),#663,.T.);
#9526=ADVANCED_FACE('',(#1201),#664,.T.);
#9527=ADVANCED_FACE('',(#1202),#665,.F.);
#9528=ADVANCED_FACE('',(#1203),#666,.T.);
#9529=ADVANCED_FACE('',(#1204),#667,.T.);
#9530=ADVANCED_FACE('',(#1205),#668,.T.);
#9531=ADVANCED_FACE('',(#1206),#669,.T.);
#9532=ADVANCED_FACE('',(#1207),#670,.F.);
#9533=ADVANCED_FACE('',(#1208),#671,.T.);
#9534=ADVANCED_FACE('',(#1209),#672,.T.);
#9535=ADVANCED_FACE('',(#1210),#673,.T.);
#9536=ADVANCED_FACE('',(#1211),#674,.T.);
#9537=ADVANCED_FACE('',(#1212),#675,.F.);
#9538=ADVANCED_FACE('',(#1213),#676,.T.);
#9539=ADVANCED_FACE('',(#1214),#677,.T.);
#9540=ADVANCED_FACE('',(#1215),#678,.T.);
#9541=ADVANCED_FACE('',(#1216),#679,.T.);
#9542=ADVANCED_FACE('',(#1217),#680,.F.);
#9543=ADVANCED_FACE('',(#1218),#681,.T.);
#9544=ADVANCED_FACE('',(#1219),#682,.T.);
#9545=ADVANCED_FACE('',(#1220),#683,.T.);
#9546=ADVANCED_FACE('',(#1221),#684,.T.);
#9547=ADVANCED_FACE('',(#1222),#685,.F.);
#9548=ADVANCED_FACE('',(#1223),#686,.T.);
#9549=ADVANCED_FACE('',(#1224),#687,.T.);
#9550=ADVANCED_FACE('',(#1225),#688,.T.);
#9551=ADVANCED_FACE('',(#1226),#689,.T.);
#9552=ADVANCED_FACE('',(#1227),#690,.F.);
#9553=ADVANCED_FACE('',(#1228),#691,.T.);
#9554=ADVANCED_FACE('',(#1229),#692,.T.);
#9555=ADVANCED_FACE('',(#1230),#693,.T.);
#9556=ADVANCED_FACE('',(#1231),#694,.T.);
#9557=ADVANCED_FACE('',(#1232),#695,.F.);
#9558=ADVANCED_FACE('',(#1233),#696,.T.);
#9559=ADVANCED_FACE('',(#1234),#697,.T.);
#9560=ADVANCED_FACE('',(#1235),#698,.T.);
#9561=ADVANCED_FACE('',(#1236),#699,.T.);
#9562=ADVANCED_FACE('',(#1237),#700,.F.);
#9563=ADVANCED_FACE('',(#1238),#701,.T.);
#9564=ADVANCED_FACE('',(#1239),#702,.T.);
#9565=ADVANCED_FACE('',(#1240),#703,.T.);
#9566=ADVANCED_FACE('',(#1241),#704,.T.);
#9567=ADVANCED_FACE('',(#1242),#705,.F.);
#9568=ADVANCED_FACE('',(#1243),#706,.T.);
#9569=ADVANCED_FACE('',(#1244),#707,.T.);
#9570=ADVANCED_FACE('',(#1245),#708,.T.);
#9571=ADVANCED_FACE('',(#1246),#709,.T.);
#9572=ADVANCED_FACE('',(#1247),#710,.F.);
#9573=ADVANCED_FACE('',(#1248),#711,.T.);
#9574=ADVANCED_FACE('',(#1249),#712,.T.);
#9575=ADVANCED_FACE('',(#1250),#713,.T.);
#9576=ADVANCED_FACE('',(#1251),#714,.T.);
#9577=ADVANCED_FACE('',(#1252),#715,.F.);
#9578=ADVANCED_FACE('',(#1253),#716,.T.);
#9579=ADVANCED_FACE('',(#1254),#717,.T.);
#9580=ADVANCED_FACE('',(#1255),#718,.T.);
#9581=ADVANCED_FACE('',(#1256),#719,.T.);
#9582=ADVANCED_FACE('',(#1257),#720,.F.);
#9583=ADVANCED_FACE('',(#1258),#721,.T.);
#9584=ADVANCED_FACE('',(#1259),#722,.T.);
#9585=ADVANCED_FACE('',(#1260),#723,.T.);
#9586=ADVANCED_FACE('',(#1261),#724,.T.);
#9587=ADVANCED_FACE('',(#1262),#725,.F.);
#9588=ADVANCED_FACE('',(#1263),#726,.T.);
#9589=ADVANCED_FACE('',(#1264),#727,.T.);
#9590=ADVANCED_FACE('',(#1265),#728,.T.);
#9591=ADVANCED_FACE('',(#1266),#729,.T.);
#9592=ADVANCED_FACE('',(#1267),#730,.F.);
#9593=ADVANCED_FACE('',(#1268),#731,.T.);
#9594=ADVANCED_FACE('',(#1269),#732,.T.);
#9595=ADVANCED_FACE('',(#1270),#733,.T.);
#9596=ADVANCED_FACE('',(#1271),#734,.T.);
#9597=ADVANCED_FACE('',(#1272),#735,.F.);
#9598=ADVANCED_FACE('',(#1273),#736,.T.);
#9599=ADVANCED_FACE('',(#1274),#737,.T.);
#9600=ADVANCED_FACE('',(#1275),#738,.T.);
#9601=ADVANCED_FACE('',(#1276),#739,.T.);
#9602=ADVANCED_FACE('',(#1277),#740,.F.);
#9603=ADVANCED_FACE('',(#1278),#741,.T.);
#9604=ADVANCED_FACE('',(#1279),#742,.T.);
#9605=ADVANCED_FACE('',(#1280),#743,.T.);
#9606=ADVANCED_FACE('',(#1281),#744,.T.);
#9607=ADVANCED_FACE('',(#1282),#745,.F.);
#9608=ADVANCED_FACE('',(#1283),#746,.T.);
#9609=ADVANCED_FACE('',(#1284),#747,.T.);
#9610=ADVANCED_FACE('',(#1285),#748,.T.);
#9611=ADVANCED_FACE('',(#1286),#749,.T.);
#9612=ADVANCED_FACE('',(#1287),#750,.F.);
#9613=ADVANCED_FACE('',(#1288),#751,.T.);
#9614=ADVANCED_FACE('',(#1289),#752,.T.);
#9615=ADVANCED_FACE('',(#1290),#753,.T.);
#9616=ADVANCED_FACE('',(#1291),#754,.T.);
#9617=ADVANCED_FACE('',(#1292),#755,.F.);
#9618=ADVANCED_FACE('',(#1293),#756,.T.);
#9619=ADVANCED_FACE('',(#1294),#757,.T.);
#9620=ADVANCED_FACE('',(#1295),#758,.T.);
#9621=ADVANCED_FACE('',(#1296),#759,.T.);
#9622=ADVANCED_FACE('',(#1297),#760,.F.);
#9623=ADVANCED_FACE('',(#1298),#761,.T.);
#9624=ADVANCED_FACE('',(#1299),#762,.T.);
#9625=ADVANCED_FACE('',(#1300),#763,.T.);
#9626=ADVANCED_FACE('',(#1301),#764,.T.);
#9627=ADVANCED_FACE('',(#1302),#765,.F.);
#9628=ADVANCED_FACE('',(#1303),#766,.T.);
#9629=ADVANCED_FACE('',(#1304),#767,.T.);
#9630=ADVANCED_FACE('',(#1305),#768,.T.);
#9631=ADVANCED_FACE('',(#1306),#769,.T.);
#9632=ADVANCED_FACE('',(#1307),#770,.F.);
#9633=ADVANCED_FACE('',(#1308),#771,.T.);
#9634=ADVANCED_FACE('',(#1309),#772,.T.);
#9635=ADVANCED_FACE('',(#1310),#773,.T.);
#9636=ADVANCED_FACE('',(#1311),#774,.T.);
#9637=ADVANCED_FACE('',(#1312),#775,.F.);
#9638=ADVANCED_FACE('',(#1313),#776,.T.);
#9639=ADVANCED_FACE('',(#1314),#777,.T.);
#9640=ADVANCED_FACE('',(#1315),#778,.T.);
#9641=ADVANCED_FACE('',(#1316),#779,.T.);
#9642=ADVANCED_FACE('',(#1317),#780,.F.);
#9643=ADVANCED_FACE('',(#1318),#781,.T.);
#9644=ADVANCED_FACE('',(#1319),#782,.T.);
#9645=ADVANCED_FACE('',(#1320),#783,.T.);
#9646=ADVANCED_FACE('',(#1321),#784,.T.);
#9647=ADVANCED_FACE('',(#1322),#785,.F.);
#9648=ADVANCED_FACE('',(#1323),#786,.T.);
#9649=ADVANCED_FACE('',(#1324),#787,.T.);
#9650=ADVANCED_FACE('',(#1325),#788,.T.);
#9651=ADVANCED_FACE('',(#1326),#789,.T.);
#9652=ADVANCED_FACE('',(#1327),#790,.F.);
#9653=ADVANCED_FACE('',(#1328),#791,.T.);
#9654=ADVANCED_FACE('',(#1329),#792,.T.);
#9655=ADVANCED_FACE('',(#1330),#793,.T.);
#9656=ADVANCED_FACE('',(#1331),#794,.T.);
#9657=ADVANCED_FACE('',(#1332),#795,.F.);
#9658=ADVANCED_FACE('',(#1333),#796,.T.);
#9659=ADVANCED_FACE('',(#1334),#797,.T.);
#9660=ADVANCED_FACE('',(#1335),#798,.T.);
#9661=ADVANCED_FACE('',(#1336),#799,.T.);
#9662=ADVANCED_FACE('',(#1337),#800,.F.);
#9663=ADVANCED_FACE('',(#1338),#801,.T.);
#9664=ADVANCED_FACE('',(#1339),#802,.T.);
#9665=ADVANCED_FACE('',(#1340),#803,.T.);
#9666=ADVANCED_FACE('',(#1341),#804,.T.);
#9667=ADVANCED_FACE('',(#1342),#805,.F.);
#9668=ADVANCED_FACE('',(#1343),#806,.T.);
#9669=ADVANCED_FACE('',(#1344),#807,.T.);
#9670=ADVANCED_FACE('',(#1345),#808,.T.);
#9671=ADVANCED_FACE('',(#1346),#809,.T.);
#9672=ADVANCED_FACE('',(#1347),#810,.F.);
#9673=ADVANCED_FACE('',(#1348),#811,.T.);
#9674=ADVANCED_FACE('',(#1349),#812,.T.);
#9675=ADVANCED_FACE('',(#1350),#813,.T.);
#9676=ADVANCED_FACE('',(#1351),#814,.T.);
#9677=ADVANCED_FACE('',(#1352),#815,.F.);
#9678=ADVANCED_FACE('',(#1353),#816,.T.);
#9679=ADVANCED_FACE('',(#1354),#817,.T.);
#9680=ADVANCED_FACE('',(#1355),#818,.T.);
#9681=ADVANCED_FACE('',(#1356),#819,.T.);
#9682=ADVANCED_FACE('',(#1357),#820,.F.);
#9683=ADVANCED_FACE('',(#1358),#821,.T.);
#9684=ADVANCED_FACE('',(#1359),#822,.T.);
#9685=ADVANCED_FACE('',(#1360),#823,.T.);
#9686=ADVANCED_FACE('',(#1361),#824,.T.);
#9687=ADVANCED_FACE('',(#1362),#825,.F.);
#9688=ADVANCED_FACE('',(#1363),#826,.T.);
#9689=ADVANCED_FACE('',(#1364),#827,.T.);
#9690=ADVANCED_FACE('',(#1365),#828,.T.);
#9691=ADVANCED_FACE('',(#1366),#829,.T.);
#9692=ADVANCED_FACE('',(#1367),#830,.F.);
#9693=ADVANCED_FACE('',(#1368),#831,.T.);
#9694=ADVANCED_FACE('',(#1369),#832,.T.);
#9695=ADVANCED_FACE('',(#1370),#833,.T.);
#9696=ADVANCED_FACE('',(#1371),#834,.T.);
#9697=ADVANCED_FACE('',(#1372),#835,.F.);
#9698=ADVANCED_FACE('',(#1373),#836,.T.);
#9699=ADVANCED_FACE('',(#1374),#837,.T.);
#9700=ADVANCED_FACE('',(#1375),#838,.T.);
#9701=ADVANCED_FACE('',(#1376),#839,.T.);
#9702=ADVANCED_FACE('',(#1377),#840,.F.);
#9703=ADVANCED_FACE('',(#1378),#841,.T.);
#9704=ADVANCED_FACE('',(#1379),#842,.T.);
#9705=ADVANCED_FACE('',(#1380),#843,.T.);
#9706=ADVANCED_FACE('',(#1381),#844,.T.);
#9707=ADVANCED_FACE('',(#1382),#845,.F.);
#9708=ADVANCED_FACE('',(#1383),#846,.T.);
#9709=ADVANCED_FACE('',(#1384),#847,.T.);
#9710=ADVANCED_FACE('',(#1385),#848,.T.);
#9711=ADVANCED_FACE('',(#1386),#849,.T.);
#9712=ADVANCED_FACE('',(#1387),#850,.F.);
#9713=ADVANCED_FACE('',(#1388),#851,.T.);
#9714=ADVANCED_FACE('',(#1389),#852,.T.);
#9715=ADVANCED_FACE('',(#1390),#9224,.F.);
#9716=ADVANCED_FACE('',(#1391),#9225,.F.);
#9717=ADVANCED_FACE('',(#1392,#415,#416),#853,.T.);
#9718=ADVANCED_FACE('',(#1393,#417,#418),#854,.F.);
#9719=ADVANCED_FACE('',(#1394),#855,.F.);
#9720=ADVANCED_FACE('',(#1395),#856,.F.);
#9721=ADVANCED_FACE('',(#1396),#857,.F.);
#9722=ADVANCED_FACE('',(#1397),#858,.F.);
#9723=ADVANCED_FACE('',(#1398),#859,.F.);
#9724=ADVANCED_FACE('',(#1399),#860,.F.);
#9725=ADVANCED_FACE('',(#1400),#861,.F.);
#9726=ADVANCED_FACE('',(#1401),#862,.F.);
#9727=ADVANCED_FACE('',(#1402),#863,.F.);
#9728=ADVANCED_FACE('',(#1403),#864,.F.);
#9729=ADVANCED_FACE('',(#1404),#865,.F.);
#9730=ADVANCED_FACE('',(#1405),#866,.F.);
#9731=ADVANCED_FACE('',(#1406),#867,.F.);
#9732=ADVANCED_FACE('',(#1407),#868,.F.);
#9733=ADVANCED_FACE('',(#1408),#187,.T.);
#9734=ADVANCED_FACE('',(#1409),#9226,.T.);
#9735=ADVANCED_FACE('',(#1410),#188,.T.);
#9736=ADVANCED_FACE('',(#1411),#9227,.F.);
#9737=ADVANCED_FACE('',(#1412,#419),#869,.F.);
#9738=ADVANCED_FACE('',(#1413,#420),#870,.F.);
#9739=ADVANCED_FACE('',(#1414),#9228,.T.);
#9740=ADVANCED_FACE('',(#1415),#9229,.T.);
#9741=ADVANCED_FACE('',(#1416),#871,.F.);
#9742=ADVANCED_FACE('',(#1417),#872,.T.);
#9743=ADVANCED_FACE('',(#1418,#421),#873,.F.);
#9744=ADVANCED_FACE('',(#1419),#9230,.F.);
#9745=ADVANCED_FACE('',(#1420,#422),#874,.T.);
#9746=ADVANCED_FACE('',(#1421,#423),#875,.F.);
#9747=ADVANCED_FACE('',(#1422),#876,.F.);
#9748=ADVANCED_FACE('',(#1423),#877,.F.);
#9749=ADVANCED_FACE('',(#1424),#878,.F.);
#9750=ADVANCED_FACE('',(#1425),#879,.F.);
#9751=ADVANCED_FACE('',(#1426),#880,.F.);
#9752=ADVANCED_FACE('',(#1427),#881,.F.);
#9753=ADVANCED_FACE('',(#1428),#9231,.T.);
#9754=ADVANCED_FACE('',(#1429),#9232,.T.);
#9755=ADVANCED_FACE('',(#1430,#424),#882,.F.);
#9756=ADVANCED_FACE('',(#1431,#425),#883,.T.);
#9757=ADVANCED_FACE('',(#1432),#884,.T.);
#9758=ADVANCED_FACE('',(#1433),#885,.T.);
#9759=ADVANCED_FACE('',(#1434),#886,.T.);
#9760=ADVANCED_FACE('',(#1435),#887,.T.);
#9761=ADVANCED_FACE('',(#1436),#888,.T.);
#9762=ADVANCED_FACE('',(#1437),#889,.T.);
#9763=ADVANCED_FACE('',(#1438),#890,.T.);
#9764=ADVANCED_FACE('',(#1439),#891,.F.);
#9765=ADVANCED_FACE('',(#1440),#9233,.T.);
#9766=ADVANCED_FACE('',(#1441),#892,.F.);
#9767=ADVANCED_FACE('',(#1442),#893,.F.);
#9768=ADVANCED_FACE('',(#1443),#894,.F.);
#9769=ADVANCED_FACE('',(#1444),#895,.F.);
#9770=ADVANCED_FACE('',(#1445),#896,.F.);
#9771=ADVANCED_FACE('',(#1446),#897,.F.);
#9772=ADVANCED_FACE('',(#1447,#426),#898,.T.);
#9773=ADVANCED_FACE('',(#1448),#899,.F.);
#9774=ADVANCED_FACE('',(#1449),#900,.T.);
#9775=ADVANCED_FACE('',(#1450),#9234,.T.);
#9776=ADVANCED_FACE('',(#1451),#9235,.T.);
#9777=ADVANCED_FACE('',(#1452,#427),#901,.F.);
#9778=ADVANCED_FACE('',(#1453,#428),#902,.T.);
#9779=ADVANCED_FACE('',(#1454),#903,.T.);
#9780=ADVANCED_FACE('',(#1455),#904,.T.);
#9781=ADVANCED_FACE('',(#1456),#905,.T.);
#9782=ADVANCED_FACE('',(#1457),#906,.T.);
#9783=ADVANCED_FACE('',(#1458),#907,.T.);
#9784=ADVANCED_FACE('',(#1459),#908,.T.);
#9785=ADVANCED_FACE('',(#1460),#909,.T.);
#9786=ADVANCED_FACE('',(#1461),#910,.F.);
#9787=CLOSED_SHELL('',(#9236,#9237,#9238,#9239,#9240,#9241,#9242,#9243,
#9244,#9245,#9246,#9247,#9248,#9249,#9250,#9251,#9252,#9253,#9254,#9255,
#9256,#9257,#9258,#9259,#9260,#9261,#9262,#9263,#9264,#9265,#9266,#9267,
#9268,#9269,#9270,#9271,#9272,#9273,#9274,#9275,#9276,#9277,#9278,#9279,
#9280,#9281,#9282,#9283));
#9788=CLOSED_SHELL('',(#9284,#9285,#9286,#9287,#9288,#9289,#9290,#9291,
#9292,#9293,#9294,#9295,#9296,#9297,#9298,#9299,#9300,#9301,#9302,#9303,
#9304,#9305,#9306,#9307,#9308,#9309,#9310,#9311,#9312,#9313,#9314,#9315,
#9316,#9317,#9318,#9319,#9320,#9321));
#9789=CLOSED_SHELL('',(#9322,#9323,#9324,#9325,#9326,#9327,#9328,#9329,
#9330,#9331,#9332,#9333,#9334,#9335,#9336,#9337,#9338,#9339,#9340,#9341,
#9342,#9343,#9344,#9345,#9346,#9347,#9348,#9349,#9350,#9351,#9352,#9353,
#9354,#9355,#9356,#9357,#9358,#9359,#9360,#9361,#9362,#9363,#9364,#9365,
#9366,#9367,#9368,#9369,#9370,#9371,#9372,#9373,#9374,#9375,#9376,#9377,
#9378,#9379));
#9790=CLOSED_SHELL('',(#9380,#9381,#9382,#9383,#9384,#9385,#9386,#9387,
#9388,#9389,#9390,#9391,#9392,#9393,#9394,#9395,#9396,#9397,#9398,#9399,
#9400,#9401));
#9791=CLOSED_SHELL('',(#9402,#9403,#9404,#9405,#9406,#9407));
#9792=CLOSED_SHELL('',(#9408,#9409,#9410,#9411,#9412,#9413));
#9793=CLOSED_SHELL('',(#9414,#9415,#9416,#9417,#9418,#9419,#9420,#9421,
#9422,#9423,#9424,#9425));
#9794=CLOSED_SHELL('',(#9426,#9427,#9428,#9429,#9430,#9431,#9432,#9433,
#9434,#9435,#9436));
#9795=CLOSED_SHELL('',(#9437,#9438,#9439,#9440,#9441,#9442,#9443,#9444,
#9445,#9446,#9447));
#9796=CLOSED_SHELL('',(#9448,#9449,#9450,#9451,#9452,#9453,#9454,#9455,
#9456,#9457,#9458,#9459,#9460));
#9797=CLOSED_SHELL('',(#9461,#9462,#9463,#9464,#9465,#9466,#9467));
#9798=CLOSED_SHELL('',(#9468,#9469,#9470,#9471,#9472,#9473,#9474));
#9799=CLOSED_SHELL('',(#9475,#9476,#9477,#9478,#9479,#9480,#9481,#9482));
#9800=CLOSED_SHELL('',(#9483,#9484,#9485));
#9801=CLOSED_SHELL('',(#9486,#9487,#9488,#9489,#9490,#9491,#9492,#9493,
#9494,#9495,#9496,#9497));
#9802=CLOSED_SHELL('',(#9498,#9499,#9500,#9501,#9502,#9503,#9504,#9505,
#9506,#9507,#9508,#9509,#9510));
#9803=CLOSED_SHELL('',(#9511,#9512,#9513,#9514,#9515,#9516,#9517,#9518,
#9519,#9520,#9521,#9522,#9523,#9524,#9525,#9526,#9527,#9528,#9529,#9530,
#9531,#9532,#9533,#9534,#9535,#9536,#9537,#9538,#9539,#9540,#9541,#9542,
#9543,#9544,#9545,#9546,#9547,#9548,#9549,#9550,#9551,#9552,#9553,#9554,
#9555,#9556,#9557,#9558,#9559,#9560,#9561,#9562,#9563,#9564,#9565,#9566,
#9567,#9568,#9569,#9570,#9571,#9572,#9573,#9574,#9575,#9576,#9577,#9578,
#9579,#9580,#9581,#9582,#9583,#9584,#9585,#9586,#9587,#9588,#9589,#9590,
#9591,#9592,#9593,#9594,#9595,#9596,#9597,#9598,#9599,#9600,#9601,#9602,
#9603,#9604,#9605,#9606,#9607,#9608,#9609,#9610,#9611,#9612,#9613,#9614,
#9615,#9616,#9617,#9618,#9619,#9620,#9621,#9622,#9623,#9624,#9625,#9626,
#9627,#9628,#9629,#9630,#9631,#9632,#9633,#9634,#9635,#9636,#9637,#9638,
#9639,#9640,#9641,#9642,#9643,#9644,#9645,#9646,#9647,#9648,#9649,#9650,
#9651,#9652,#9653,#9654,#9655,#9656,#9657,#9658,#9659,#9660,#9661,#9662,
#9663,#9664,#9665,#9666,#9667,#9668,#9669,#9670,#9671,#9672,#9673,#9674,
#9675,#9676,#9677,#9678,#9679,#9680,#9681,#9682,#9683,#9684,#9685,#9686,
#9687,#9688,#9689,#9690,#9691,#9692,#9693,#9694,#9695,#9696,#9697,#9698,
#9699,#9700,#9701,#9702,#9703,#9704,#9705,#9706,#9707,#9708,#9709,#9710,
#9711,#9712,#9713,#9714));
#9804=CLOSED_SHELL('',(#9715,#9716,#9717,#9718,#9719,#9720,#9721,#9722,
#9723,#9724,#9725,#9726,#9727,#9728,#9729,#9730,#9731,#9732));
#9805=CLOSED_SHELL('',(#9733,#9734,#9735,#9736,#9737,#9738));
#9806=CLOSED_SHELL('',(#9739,#9740,#9741,#9742,#9743));
#9807=CLOSED_SHELL('',(#9744,#9745,#9746,#9747,#9748,#9749,#9750,#9751,
#9752));
#9808=CLOSED_SHELL('',(#9753,#9754,#9755,#9756,#9757,#9758,#9759,#9760,
#9761,#9762,#9763,#9764));
#9809=CLOSED_SHELL('',(#9765,#9766,#9767,#9768,#9769,#9770,#9771,#9772,
#9773,#9774));
#9810=CLOSED_SHELL('',(#9775,#9776,#9777,#9778,#9779,#9780,#9781,#9782,
#9783,#9784,#9785,#9786));
#9811=DERIVED_UNIT_ELEMENT(#9859,1.);
#9812=DERIVED_UNIT_ELEMENT(#16600,-3.);
#9813=DERIVED_UNIT_ELEMENT(#9859,1.);
#9814=DERIVED_UNIT_ELEMENT(#16600,-3.);
#9815=DERIVED_UNIT_ELEMENT(#9859,1.);
#9816=DERIVED_UNIT_ELEMENT(#16600,-3.);
#9817=DERIVED_UNIT_ELEMENT(#9859,1.);
#9818=DERIVED_UNIT_ELEMENT(#16600,-3.);
#9819=DERIVED_UNIT_ELEMENT(#9859,1.);
#9820=DERIVED_UNIT_ELEMENT(#16600,-3.);
#9821=DERIVED_UNIT_ELEMENT(#9859,1.);
#9822=DERIVED_UNIT_ELEMENT(#16600,-3.);
#9823=DERIVED_UNIT_ELEMENT(#9859,1.);
#9824=DERIVED_UNIT_ELEMENT(#16600,-3.);
#9825=DERIVED_UNIT_ELEMENT(#9859,1.);
#9826=DERIVED_UNIT_ELEMENT(#16600,-3.);
#9827=DERIVED_UNIT_ELEMENT(#9859,1.);
#9828=DERIVED_UNIT_ELEMENT(#16600,-3.);
#9829=DERIVED_UNIT_ELEMENT(#9859,1.);
#9830=DERIVED_UNIT_ELEMENT(#16600,-3.);
#9831=DERIVED_UNIT_ELEMENT(#9859,1.);
#9832=DERIVED_UNIT_ELEMENT(#16600,-3.);
#9833=DERIVED_UNIT_ELEMENT(#9859,1.);
#9834=DERIVED_UNIT_ELEMENT(#16600,-3.);
#9835=DERIVED_UNIT_ELEMENT(#9859,1.);
#9836=DERIVED_UNIT_ELEMENT(#16600,-3.);
#9837=DERIVED_UNIT_ELEMENT(#9859,1.);
#9838=DERIVED_UNIT_ELEMENT(#16600,-3.);
#9839=DERIVED_UNIT_ELEMENT(#9859,1.);
#9840=DERIVED_UNIT_ELEMENT(#16600,-3.);
#9841=DERIVED_UNIT_ELEMENT(#9859,1.);
#9842=DERIVED_UNIT_ELEMENT(#16600,-3.);
#9843=DERIVED_UNIT_ELEMENT(#9859,1.);
#9844=DERIVED_UNIT_ELEMENT(#16600,-3.);
#9845=DERIVED_UNIT_ELEMENT(#9859,1.);
#9846=DERIVED_UNIT_ELEMENT(#16600,-3.);
#9847=DERIVED_UNIT_ELEMENT(#9859,1.);
#9848=DERIVED_UNIT_ELEMENT(#16600,-3.);
#9849=DERIVED_UNIT_ELEMENT(#9859,1.);
#9850=DERIVED_UNIT_ELEMENT(#16600,-3.);
#9851=DERIVED_UNIT_ELEMENT(#9859,1.);
#9852=DERIVED_UNIT_ELEMENT(#16600,-3.);
#9853=DERIVED_UNIT_ELEMENT(#9859,1.);
#9854=DERIVED_UNIT_ELEMENT(#16600,-3.);
#9855=DERIVED_UNIT_ELEMENT(#9859,1.);
#9856=DERIVED_UNIT_ELEMENT(#16600,-3.);
#9857=DERIVED_UNIT_ELEMENT(#9859,1.);
#9858=DERIVED_UNIT_ELEMENT(#16600,-3.);
#9859=(
MASS_UNIT()
NAMED_UNIT(*)
SI_UNIT(.KILO.,.GRAM.)
);
#9860=DERIVED_UNIT((#9811,#9812));
#9861=DERIVED_UNIT((#9813,#9814));
#9862=DERIVED_UNIT((#9815,#9816));
#9863=DERIVED_UNIT((#9817,#9818));
#9864=DERIVED_UNIT((#9819,#9820));
#9865=DERIVED_UNIT((#9821,#9822));
#9866=DERIVED_UNIT((#9823,#9824));
#9867=DERIVED_UNIT((#9825,#9826));
#9868=DERIVED_UNIT((#9827,#9828));
#9869=DERIVED_UNIT((#9829,#9830));
#9870=DERIVED_UNIT((#9831,#9832));
#9871=DERIVED_UNIT((#9833,#9834));
#9872=DERIVED_UNIT((#9835,#9836));
#9873=DERIVED_UNIT((#9837,#9838));
#9874=DERIVED_UNIT((#9839,#9840));
#9875=DERIVED_UNIT((#9841,#9842));
#9876=DERIVED_UNIT((#9843,#9844));
#9877=DERIVED_UNIT((#9845,#9846));
#9878=DERIVED_UNIT((#9847,#9848));
#9879=DERIVED_UNIT((#9849,#9850));
#9880=DERIVED_UNIT((#9851,#9852));
#9881=DERIVED_UNIT((#9853,#9854));
#9882=DERIVED_UNIT((#9855,#9856));
#9883=DERIVED_UNIT((#9857,#9858));
#9884=MEASURE_REPRESENTATION_ITEM('density measure',
POSITIVE_RATIO_MEASURE(7850.),#9860);
#9885=MEASURE_REPRESENTATION_ITEM('density measure',
POSITIVE_RATIO_MEASURE(7850.),#9861);
#9886=MEASURE_REPRESENTATION_ITEM('density measure',
POSITIVE_RATIO_MEASURE(7850.),#9862);
#9887=MEASURE_REPRESENTATION_ITEM('density measure',
POSITIVE_RATIO_MEASURE(7850.),#9863);
#9888=MEASURE_REPRESENTATION_ITEM('density measure',
POSITIVE_RATIO_MEASURE(7850.),#9864);
#9889=MEASURE_REPRESENTATION_ITEM('density measure',
POSITIVE_RATIO_MEASURE(7850.),#9865);
#9890=MEASURE_REPRESENTATION_ITEM('density measure',
POSITIVE_RATIO_MEASURE(7850.),#9866);
#9891=MEASURE_REPRESENTATION_ITEM('density measure',
POSITIVE_RATIO_MEASURE(7850.),#9867);
#9892=MEASURE_REPRESENTATION_ITEM('density measure',
POSITIVE_RATIO_MEASURE(7850.),#9868);
#9893=MEASURE_REPRESENTATION_ITEM('density measure',
POSITIVE_RATIO_MEASURE(7850.),#9869);
#9894=MEASURE_REPRESENTATION_ITEM('density measure',
POSITIVE_RATIO_MEASURE(7850.),#9870);
#9895=MEASURE_REPRESENTATION_ITEM('density measure',
POSITIVE_RATIO_MEASURE(7850.),#9871);
#9896=MEASURE_REPRESENTATION_ITEM('density measure',
POSITIVE_RATIO_MEASURE(7850.),#9872);
#9897=MEASURE_REPRESENTATION_ITEM('density measure',
POSITIVE_RATIO_MEASURE(7850.),#9873);
#9898=MEASURE_REPRESENTATION_ITEM('density measure',
POSITIVE_RATIO_MEASURE(7850.),#9874);
#9899=MEASURE_REPRESENTATION_ITEM('density measure',
POSITIVE_RATIO_MEASURE(7850.),#9875);
#9900=MEASURE_REPRESENTATION_ITEM('density measure',
POSITIVE_RATIO_MEASURE(7850.),#9876);
#9901=MEASURE_REPRESENTATION_ITEM('density measure',
POSITIVE_RATIO_MEASURE(7850.),#9877);
#9902=MEASURE_REPRESENTATION_ITEM('density measure',
POSITIVE_RATIO_MEASURE(7850.),#9878);
#9903=MEASURE_REPRESENTATION_ITEM('density measure',
POSITIVE_RATIO_MEASURE(7850.),#9879);
#9904=MEASURE_REPRESENTATION_ITEM('density measure',
POSITIVE_RATIO_MEASURE(7850.),#9880);
#9905=MEASURE_REPRESENTATION_ITEM('density measure',
POSITIVE_RATIO_MEASURE(7850.),#9881);
#9906=MEASURE_REPRESENTATION_ITEM('density measure',
POSITIVE_RATIO_MEASURE(7850.),#9882);
#9907=MEASURE_REPRESENTATION_ITEM('density measure',
POSITIVE_RATIO_MEASURE(7850.),#9883);
#9908=PROPERTY_DEFINITION_REPRESENTATION(#10028,#9956);
#9909=PROPERTY_DEFINITION_REPRESENTATION(#10029,#9957);
#9910=PROPERTY_DEFINITION_REPRESENTATION(#10030,#9958);
#9911=PROPERTY_DEFINITION_REPRESENTATION(#10031,#9959);
#9912=PROPERTY_DEFINITION_REPRESENTATION(#10032,#9960);
#9913=PROPERTY_DEFINITION_REPRESENTATION(#10033,#9961);
#9914=PROPERTY_DEFINITION_REPRESENTATION(#10034,#9962);
#9915=PROPERTY_DEFINITION_REPRESENTATION(#10035,#9963);
#9916=PROPERTY_DEFINITION_REPRESENTATION(#10036,#9964);
#9917=PROPERTY_DEFINITION_REPRESENTATION(#10037,#9965);
#9918=PROPERTY_DEFINITION_REPRESENTATION(#10038,#9966);
#9919=PROPERTY_DEFINITION_REPRESENTATION(#10039,#9967);
#9920=PROPERTY_DEFINITION_REPRESENTATION(#10040,#9968);
#9921=PROPERTY_DEFINITION_REPRESENTATION(#10041,#9969);
#9922=PROPERTY_DEFINITION_REPRESENTATION(#10042,#9970);
#9923=PROPERTY_DEFINITION_REPRESENTATION(#10043,#9971);
#9924=PROPERTY_DEFINITION_REPRESENTATION(#10044,#9972);
#9925=PROPERTY_DEFINITION_REPRESENTATION(#10045,#9973);
#9926=PROPERTY_DEFINITION_REPRESENTATION(#10046,#9974);
#9927=PROPERTY_DEFINITION_REPRESENTATION(#10047,#9975);
#9928=PROPERTY_DEFINITION_REPRESENTATION(#10048,#9976);
#9929=PROPERTY_DEFINITION_REPRESENTATION(#10049,#9977);
#9930=PROPERTY_DEFINITION_REPRESENTATION(#10050,#9978);
#9931=PROPERTY_DEFINITION_REPRESENTATION(#10051,#9979);
#9932=PROPERTY_DEFINITION_REPRESENTATION(#10052,#9980);
#9933=PROPERTY_DEFINITION_REPRESENTATION(#10053,#9981);
#9934=PROPERTY_DEFINITION_REPRESENTATION(#10054,#9982);
#9935=PROPERTY_DEFINITION_REPRESENTATION(#10055,#9983);
#9936=PROPERTY_DEFINITION_REPRESENTATION(#10056,#9984);
#9937=PROPERTY_DEFINITION_REPRESENTATION(#10057,#9985);
#9938=PROPERTY_DEFINITION_REPRESENTATION(#10058,#9986);
#9939=PROPERTY_DEFINITION_REPRESENTATION(#10059,#9987);
#9940=PROPERTY_DEFINITION_REPRESENTATION(#10060,#9988);
#9941=PROPERTY_DEFINITION_REPRESENTATION(#10061,#9989);
#9942=PROPERTY_DEFINITION_REPRESENTATION(#10062,#9990);
#9943=PROPERTY_DEFINITION_REPRESENTATION(#10063,#9991);
#9944=PROPERTY_DEFINITION_REPRESENTATION(#10064,#9992);
#9945=PROPERTY_DEFINITION_REPRESENTATION(#10065,#9993);
#9946=PROPERTY_DEFINITION_REPRESENTATION(#10066,#9994);
#9947=PROPERTY_DEFINITION_REPRESENTATION(#10067,#9995);
#9948=PROPERTY_DEFINITION_REPRESENTATION(#10068,#9996);
#9949=PROPERTY_DEFINITION_REPRESENTATION(#10069,#9997);
#9950=PROPERTY_DEFINITION_REPRESENTATION(#10070,#9998);
#9951=PROPERTY_DEFINITION_REPRESENTATION(#10071,#9999);
#9952=PROPERTY_DEFINITION_REPRESENTATION(#10072,#10000);
#9953=PROPERTY_DEFINITION_REPRESENTATION(#10073,#10001);
#9954=PROPERTY_DEFINITION_REPRESENTATION(#10074,#10002);
#9955=PROPERTY_DEFINITION_REPRESENTATION(#10075,#10003);
#9956=REPRESENTATION('material name',(#10004),#16574);
#9957=REPRESENTATION('density',(#9884),#16574);
#9958=REPRESENTATION('material name',(#10005),#16575);
#9959=REPRESENTATION('density',(#9885),#16575);
#9960=REPRESENTATION('material name',(#10006),#16576);
#9961=REPRESENTATION('density',(#9886),#16576);
#9962=REPRESENTATION('material name',(#10007),#16577);
#9963=REPRESENTATION('density',(#9887),#16577);
#9964=REPRESENTATION('material name',(#10008),#16578);
#9965=REPRESENTATION('density',(#9888),#16578);
#9966=REPRESENTATION('material name',(#10009),#16579);
#9967=REPRESENTATION('density',(#9889),#16579);
#9968=REPRESENTATION('material name',(#10010),#16580);
#9969=REPRESENTATION('density',(#9890),#16580);
#9970=REPRESENTATION('material name',(#10011),#16581);
#9971=REPRESENTATION('density',(#9891),#16581);
#9972=REPRESENTATION('material name',(#10012),#16582);
#9973=REPRESENTATION('density',(#9892),#16582);
#9974=REPRESENTATION('material name',(#10013),#16583);
#9975=REPRESENTATION('density',(#9893),#16583);
#9976=REPRESENTATION('material name',(#10014),#16584);
#9977=REPRESENTATION('density',(#9894),#16584);
#9978=REPRESENTATION('material name',(#10015),#16585);
#9979=REPRESENTATION('density',(#9895),#16585);
#9980=REPRESENTATION('material name',(#10016),#16586);
#9981=REPRESENTATION('density',(#9896),#16586);
#9982=REPRESENTATION('material name',(#10017),#16587);
#9983=REPRESENTATION('density',(#9897),#16587);
#9984=REPRESENTATION('material name',(#10018),#16588);
#9985=REPRESENTATION('density',(#9898),#16588);
#9986=REPRESENTATION('material name',(#10019),#16589);
#9987=REPRESENTATION('density',(#9899),#16589);
#9988=REPRESENTATION('material name',(#10020),#16590);
#9989=REPRESENTATION('density',(#9900),#16590);
#9990=REPRESENTATION('material name',(#10021),#16591);
#9991=REPRESENTATION('density',(#9901),#16591);
#9992=REPRESENTATION('material name',(#10022),#16592);
#9993=REPRESENTATION('density',(#9902),#16592);
#9994=REPRESENTATION('material name',(#10023),#16593);
#9995=REPRESENTATION('density',(#9903),#16593);
#9996=REPRESENTATION('material name',(#10024),#16594);
#9997=REPRESENTATION('density',(#9904),#16594);
#9998=REPRESENTATION('material name',(#10025),#16595);
#9999=REPRESENTATION('density',(#9905),#16595);
#10000=REPRESENTATION('material name',(#10026),#16596);
#10001=REPRESENTATION('density',(#9906),#16596);
#10002=REPRESENTATION('material name',(#10027),#16597);
#10003=REPRESENTATION('density',(#9907),#16597);
#10004=DESCRIPTIVE_REPRESENTATION_ITEM('Steel','Steel');
#10005=DESCRIPTIVE_REPRESENTATION_ITEM('Steel','Steel');
#10006=DESCRIPTIVE_REPRESENTATION_ITEM('Steel','Steel');
#10007=DESCRIPTIVE_REPRESENTATION_ITEM('Steel','Steel');
#10008=DESCRIPTIVE_REPRESENTATION_ITEM('Steel','Steel');
#10009=DESCRIPTIVE_REPRESENTATION_ITEM('Steel','Steel');
#10010=DESCRIPTIVE_REPRESENTATION_ITEM('Steel','Steel');
#10011=DESCRIPTIVE_REPRESENTATION_ITEM('Steel','Steel');
#10012=DESCRIPTIVE_REPRESENTATION_ITEM('Steel','Steel');
#10013=DESCRIPTIVE_REPRESENTATION_ITEM('Steel','Steel');
#10014=DESCRIPTIVE_REPRESENTATION_ITEM('Steel','Steel');
#10015=DESCRIPTIVE_REPRESENTATION_ITEM('Steel','Steel');
#10016=DESCRIPTIVE_REPRESENTATION_ITEM('Steel','Steel');
#10017=DESCRIPTIVE_REPRESENTATION_ITEM('Steel','Steel');
#10018=DESCRIPTIVE_REPRESENTATION_ITEM('Steel','Steel');
#10019=DESCRIPTIVE_REPRESENTATION_ITEM('Steel','Steel');
#10020=DESCRIPTIVE_REPRESENTATION_ITEM('Steel','Steel');
#10021=DESCRIPTIVE_REPRESENTATION_ITEM('Steel','Steel');
#10022=DESCRIPTIVE_REPRESENTATION_ITEM('Steel','Steel');
#10023=DESCRIPTIVE_REPRESENTATION_ITEM('Steel','Steel');
#10024=DESCRIPTIVE_REPRESENTATION_ITEM('Steel','Steel');
#10025=DESCRIPTIVE_REPRESENTATION_ITEM('Steel','Steel');
#10026=DESCRIPTIVE_REPRESENTATION_ITEM('Steel','Steel');
#10027=DESCRIPTIVE_REPRESENTATION_ITEM('Steel','Steel');
#10028=PROPERTY_DEFINITION('material property','material name',#16724);
#10029=PROPERTY_DEFINITION('material property','density of part',#16724);
#10030=PROPERTY_DEFINITION('material property','material name',#16725);
#10031=PROPERTY_DEFINITION('material property','density of part',#16725);
#10032=PROPERTY_DEFINITION('material property','material name',#16726);
#10033=PROPERTY_DEFINITION('material property','density of part',#16726);
#10034=PROPERTY_DEFINITION('material property','material name',#16727);
#10035=PROPERTY_DEFINITION('material property','density of part',#16727);
#10036=PROPERTY_DEFINITION('material property','material name',#16728);
#10037=PROPERTY_DEFINITION('material property','density of part',#16728);
#10038=PROPERTY_DEFINITION('material property','material name',#16729);
#10039=PROPERTY_DEFINITION('material property','density of part',#16729);
#10040=PROPERTY_DEFINITION('material property','material name',#16730);
#10041=PROPERTY_DEFINITION('material property','density of part',#16730);
#10042=PROPERTY_DEFINITION('material property','material name',#16731);
#10043=PROPERTY_DEFINITION('material property','density of part',#16731);
#10044=PROPERTY_DEFINITION('material property','material name',#16732);
#10045=PROPERTY_DEFINITION('material property','density of part',#16732);
#10046=PROPERTY_DEFINITION('material property','material name',#16733);
#10047=PROPERTY_DEFINITION('material property','density of part',#16733);
#10048=PROPERTY_DEFINITION('material property','material name',#16734);
#10049=PROPERTY_DEFINITION('material property','density of part',#16734);
#10050=PROPERTY_DEFINITION('material property','material name',#16735);
#10051=PROPERTY_DEFINITION('material property','density of part',#16735);
#10052=PROPERTY_DEFINITION('material property','material name',#16736);
#10053=PROPERTY_DEFINITION('material property','density of part',#16736);
#10054=PROPERTY_DEFINITION('material property','material name',#16737);
#10055=PROPERTY_DEFINITION('material property','density of part',#16737);
#10056=PROPERTY_DEFINITION('material property','material name',#16738);
#10057=PROPERTY_DEFINITION('material property','density of part',#16738);
#10058=PROPERTY_DEFINITION('material property','material name',#16739);
#10059=PROPERTY_DEFINITION('material property','density of part',#16739);
#10060=PROPERTY_DEFINITION('material property','material name',#16740);
#10061=PROPERTY_DEFINITION('material property','density of part',#16740);
#10062=PROPERTY_DEFINITION('material property','material name',#16741);
#10063=PROPERTY_DEFINITION('material property','density of part',#16741);
#10064=PROPERTY_DEFINITION('material property','material name',#16742);
#10065=PROPERTY_DEFINITION('material property','density of part',#16742);
#10066=PROPERTY_DEFINITION('material property','material name',#16743);
#10067=PROPERTY_DEFINITION('material property','density of part',#16743);
#10068=PROPERTY_DEFINITION('material property','material name',#16744);
#10069=PROPERTY_DEFINITION('material property','density of part',#16744);
#10070=PROPERTY_DEFINITION('material property','material name',#16745);
#10071=PROPERTY_DEFINITION('material property','density of part',#16745);
#10072=PROPERTY_DEFINITION('material property','material name',#16746);
#10073=PROPERTY_DEFINITION('material property','density of part',#16746);
#10074=PROPERTY_DEFINITION('material property','material name',#16747);
#10075=PROPERTY_DEFINITION('material property','density of part',#16747);
#10076=AXIS2_PLACEMENT_3D('',#13680,#10928,#10929);
#10077=AXIS2_PLACEMENT_3D('',#13681,#10930,#10931);
#10078=AXIS2_PLACEMENT_3D('',#13682,#10932,#10933);
#10079=AXIS2_PLACEMENT_3D('',#13684,#10934,#10935);
#10080=AXIS2_PLACEMENT_3D('',#13687,#10937,#10938);
#10081=AXIS2_PLACEMENT_3D('',#13688,#10939,#10940);
#10082=AXIS2_PLACEMENT_3D('',#13690,#10941,#10942);
#10083=AXIS2_PLACEMENT_3D('',#13693,#10944,#10945);
#10084=AXIS2_PLACEMENT_3D('',#13694,#10946,#10947);
#10085=AXIS2_PLACEMENT_3D('',#13775,#10988,#10989);
#10086=AXIS2_PLACEMENT_3D('',#13781,#10993,#10994);
#10087=AXIS2_PLACEMENT_3D('',#13787,#10998,#10999);
#10088=AXIS2_PLACEMENT_3D('',#13793,#11003,#11004);
#10089=AXIS2_PLACEMENT_3D('',#13799,#11008,#11009);
#10090=AXIS2_PLACEMENT_3D('',#13805,#11013,#11014);
#10091=AXIS2_PLACEMENT_3D('',#13811,#11018,#11019);
#10092=AXIS2_PLACEMENT_3D('',#13817,#11023,#11024);
#10093=AXIS2_PLACEMENT_3D('',#13823,#11028,#11029);
#10094=AXIS2_PLACEMENT_3D('',#13856,#11050,#11051);
#10095=AXIS2_PLACEMENT_3D('',#13857,#11052,#11053);
#10096=AXIS2_PLACEMENT_3D('',#13858,#11054,#11055);
#10097=AXIS2_PLACEMENT_3D('',#13859,#11056,#11057);
#10098=AXIS2_PLACEMENT_3D('',#13865,#11061,#11062);
#10099=AXIS2_PLACEMENT_3D('',#13871,#11066,#11067);
#10100=AXIS2_PLACEMENT_3D('',#13877,#11071,#11072);
#10101=AXIS2_PLACEMENT_3D('',#13880,#11075,#11076);
#10102=AXIS2_PLACEMENT_3D('',#13881,#11077,#11078);
#10103=AXIS2_PLACEMENT_3D('',#13882,#11079,#11080);
#10104=AXIS2_PLACEMENT_3D('',#13888,#11084,#11085);
#10105=AXIS2_PLACEMENT_3D('',#13894,#11089,#11090);
#10106=AXIS2_PLACEMENT_3D('',#13900,#11094,#11095);
#10107=AXIS2_PLACEMENT_3D('',#13903,#11098,#11099);
#10108=AXIS2_PLACEMENT_3D('',#13904,#11100,#11101);
#10109=AXIS2_PLACEMENT_3D('',#13905,#11102,#11103);
#10110=AXIS2_PLACEMENT_3D('',#13907,#11105,#11106);
#10111=AXIS2_PLACEMENT_3D('',#13909,#11108,#11109);
#10112=AXIS2_PLACEMENT_3D('',#13910,#11110,#11111);
#10113=AXIS2_PLACEMENT_3D('',#13912,#11113,#11114);
#10114=AXIS2_PLACEMENT_3D('',#13914,#11116,#11117);
#10115=AXIS2_PLACEMENT_3D('',#13915,#11118,#11119);
#10116=AXIS2_PLACEMENT_3D('',#13917,#11121,#11122);
#10117=AXIS2_PLACEMENT_3D('',#13919,#11124,#11125);
#10118=AXIS2_PLACEMENT_3D('',#13920,#11126,#11127);
#10119=AXIS2_PLACEMENT_3D('',#13922,#11129,#11130);
#10120=AXIS2_PLACEMENT_3D('',#13924,#11132,#11133);
#10121=AXIS2_PLACEMENT_3D('',#13925,#11134,#11135);
#10122=AXIS2_PLACEMENT_3D('',#13927,#11137,#11138);
#10123=AXIS2_PLACEMENT_3D('',#13929,#11140,#11141);
#10124=AXIS2_PLACEMENT_3D('',#13930,#11142,#11143);
#10125=AXIS2_PLACEMENT_3D('',#13932,#11145,#11146);
#10126=AXIS2_PLACEMENT_3D('',#13934,#11148,#11149);
#10127=AXIS2_PLACEMENT_3D('',#13935,#11150,#11151);
#10128=AXIS2_PLACEMENT_3D('',#13936,#11152,#11153);
#10129=AXIS2_PLACEMENT_3D('',#13937,#11154,#11155);
#10130=AXIS2_PLACEMENT_3D('',#13938,#11156,#11157);
#10131=AXIS2_PLACEMENT_3D('',#13939,#11158,#11159);
#10132=AXIS2_PLACEMENT_3D('',#13940,#11160,#11161);
#10133=AXIS2_PLACEMENT_3D('',#13941,#11162,#11163);
#10134=AXIS2_PLACEMENT_3D('',#13944,#11164,#11165);
#10135=AXIS2_PLACEMENT_3D('',#13948,#11167,#11168);
#10136=AXIS2_PLACEMENT_3D('',#13950,#11170,#11171);
#10137=AXIS2_PLACEMENT_3D('',#13952,#11172,#11173);
#10138=AXIS2_PLACEMENT_3D('',#13955,#11175,#11176);
#10139=AXIS2_PLACEMENT_3D('',#13956,#11177,#11178);
#10140=AXIS2_PLACEMENT_3D('',#13958,#11179,#11180);
#10141=AXIS2_PLACEMENT_3D('',#13961,#11182,#11183);
#10142=AXIS2_PLACEMENT_3D('',#13962,#11184,#11185);
#10143=AXIS2_PLACEMENT_3D('',#13964,#11186,#11187);
#10144=AXIS2_PLACEMENT_3D('',#13968,#11189,#11190);
#10145=AXIS2_PLACEMENT_3D('',#13970,#11191,#11192);
#10146=AXIS2_PLACEMENT_3D('',#13971,#11193,#11194);
#10147=AXIS2_PLACEMENT_3D('',#13972,#11195,#11196);
#10148=AXIS2_PLACEMENT_3D('',#13974,#11197,#11198);
#10149=AXIS2_PLACEMENT_3D('',#13978,#11200,#11201);
#10150=AXIS2_PLACEMENT_3D('',#13980,#11202,#11203);
#10151=AXIS2_PLACEMENT_3D('',#13981,#11204,#11205);
#10152=AXIS2_PLACEMENT_3D('',#13982,#11206,#11207);
#10153=AXIS2_PLACEMENT_3D('',#13984,#11208,#11209);
#10154=AXIS2_PLACEMENT_3D('',#13988,#11211,#11212);
#10155=AXIS2_PLACEMENT_3D('',#13990,#11213,#11214);
#10156=AXIS2_PLACEMENT_3D('',#13991,#11215,#11216);
#10157=AXIS2_PLACEMENT_3D('',#13992,#11217,#11218);
#10158=AXIS2_PLACEMENT_3D('',#14019,#11233,#11234);
#10159=AXIS2_PLACEMENT_3D('',#14031,#11242,#11243);
#10160=AXIS2_PLACEMENT_3D('',#14037,#11247,#11248);
#10161=AXIS2_PLACEMENT_3D('',#14043,#11252,#11253);
#10162=AXIS2_PLACEMENT_3D('',#14049,#11257,#11258);
#10163=AXIS2_PLACEMENT_3D('',#14055,#11262,#11263);
#10164=AXIS2_PLACEMENT_3D('',#14061,#11267,#11268);
#10165=AXIS2_PLACEMENT_3D('',#14064,#11271,#11272);
#10166=AXIS2_PLACEMENT_3D('',#14070,#11276,#11277);
#10167=AXIS2_PLACEMENT_3D('',#14076,#11281,#11282);
#10168=AXIS2_PLACEMENT_3D('',#14082,#11286,#11287);
#10169=AXIS2_PLACEMENT_3D('',#14085,#11290,#11291);
#10170=AXIS2_PLACEMENT_3D('',#14086,#11292,#11293);
#10171=AXIS2_PLACEMENT_3D('',#14087,#11294,#11295);
#10172=AXIS2_PLACEMENT_3D('',#14093,#11299,#11300);
#10173=AXIS2_PLACEMENT_3D('',#14099,#11304,#11305);
#10174=AXIS2_PLACEMENT_3D('',#14105,#11309,#11310);
#10175=AXIS2_PLACEMENT_3D('',#14108,#11313,#11314);
#10176=AXIS2_PLACEMENT_3D('',#14109,#11315,#11316);
#10177=AXIS2_PLACEMENT_3D('',#14110,#11317,#11318);
#10178=AXIS2_PLACEMENT_3D('',#14116,#11322,#11323);
#10179=AXIS2_PLACEMENT_3D('',#14122,#11327,#11328);
#10180=AXIS2_PLACEMENT_3D('',#14128,#11332,#11333);
#10181=AXIS2_PLACEMENT_3D('',#14131,#11336,#11337);
#10182=AXIS2_PLACEMENT_3D('',#14132,#11338,#11339);
#10183=AXIS2_PLACEMENT_3D('',#14133,#11340,#11341);
#10184=AXIS2_PLACEMENT_3D('',#14134,#11342,#11343);
#10185=AXIS2_PLACEMENT_3D('',#14135,#11344,#11345);
#10186=AXIS2_PLACEMENT_3D('',#14136,#11346,#11347);
#10187=AXIS2_PLACEMENT_3D('',#14137,#11348,#11349);
#10188=AXIS2_PLACEMENT_3D('',#14138,#11350,#11351);
#10189=AXIS2_PLACEMENT_3D('',#14139,#11352,#11353);
#10190=AXIS2_PLACEMENT_3D('',#14140,#11354,#11355);
#10191=AXIS2_PLACEMENT_3D('',#14142,#11356,#11357);
#10192=AXIS2_PLACEMENT_3D('',#14146,#11359,#11360);
#10193=AXIS2_PLACEMENT_3D('',#14148,#11361,#11362);
#10194=AXIS2_PLACEMENT_3D('',#14149,#11363,#11364);
#10195=AXIS2_PLACEMENT_3D('',#14150,#11365,#11366);
#10196=AXIS2_PLACEMENT_3D('',#14152,#11367,#11368);
#10197=AXIS2_PLACEMENT_3D('',#14156,#11370,#11371);
#10198=AXIS2_PLACEMENT_3D('',#14158,#11372,#11373);
#10199=AXIS2_PLACEMENT_3D('',#14159,#11374,#11375);
#10200=AXIS2_PLACEMENT_3D('',#14160,#11376,#11377);
#10201=AXIS2_PLACEMENT_3D('',#14162,#11378,#11379);
#10202=AXIS2_PLACEMENT_3D('',#14166,#11381,#11382);
#10203=AXIS2_PLACEMENT_3D('',#14168,#11383,#11384);
#10204=AXIS2_PLACEMENT_3D('',#14169,#11385,#11386);
#10205=AXIS2_PLACEMENT_3D('',#14170,#11387,#11388);
#10206=AXIS2_PLACEMENT_3D('',#14172,#11389,#11390);
#10207=AXIS2_PLACEMENT_3D('',#14175,#11392,#11393);
#10208=AXIS2_PLACEMENT_3D('',#14176,#11394,#11395);
#10209=AXIS2_PLACEMENT_3D('',#14178,#11396,#11397);
#10210=AXIS2_PLACEMENT_3D('',#14181,#11399,#11400);
#10211=AXIS2_PLACEMENT_3D('',#14182,#11401,#11402);
#10212=AXIS2_PLACEMENT_3D('',#14184,#11403,#11404);
#10213=AXIS2_PLACEMENT_3D('',#14187,#11406,#11407);
#10214=AXIS2_PLACEMENT_3D('',#14188,#11408,#11409);
#10215=AXIS2_PLACEMENT_3D('',#14237,#11434,#11435);
#10216=AXIS2_PLACEMENT_3D('',#14262,#11448,#11449);
#10217=AXIS2_PLACEMENT_3D('',#14273,#11456,#11457);
#10218=AXIS2_PLACEMENT_3D('',#14279,#11461,#11462);
#10219=AXIS2_PLACEMENT_3D('',#14285,#11466,#11467);
#10220=AXIS2_PLACEMENT_3D('',#14291,#11471,#11472);
#10221=AXIS2_PLACEMENT_3D('',#14297,#11476,#11477);
#10222=AXIS2_PLACEMENT_3D('',#14303,#11481,#11482);
#10223=AXIS2_PLACEMENT_3D('',#14309,#11486,#11487);
#10224=AXIS2_PLACEMENT_3D('',#14318,#11492,#11493);
#10225=AXIS2_PLACEMENT_3D('',#14327,#11498,#11499);
#10226=AXIS2_PLACEMENT_3D('',#14333,#11503,#11504);
#10227=AXIS2_PLACEMENT_3D('',#14339,#11508,#11509);
#10228=AXIS2_PLACEMENT_3D('',#14348,#11516,#11517);
#10229=AXIS2_PLACEMENT_3D('',#14357,#11523,#11524);
#10230=AXIS2_PLACEMENT_3D('',#14359,#11526,#11527);
#10231=AXIS2_PLACEMENT_3D('',#14363,#11530,#11531);
#10232=AXIS2_PLACEMENT_3D('',#14367,#11534,#11535);
#10233=AXIS2_PLACEMENT_3D('',#14371,#11538,#11539);
#10234=AXIS2_PLACEMENT_3D('',#14378,#11544,#11545);
#10235=AXIS2_PLACEMENT_3D('',#14380,#11547,#11548);
#10236=AXIS2_PLACEMENT_3D('',#14390,#11554,#11555);
#10237=AXIS2_PLACEMENT_3D('',#14392,#11557,#11558);
#10238=AXIS2_PLACEMENT_3D('',#14402,#11564,#11565);
#10239=AXIS2_PLACEMENT_3D('',#14406,#11568,#11569);
#10240=AXIS2_PLACEMENT_3D('',#14410,#11572,#11573);
#10241=AXIS2_PLACEMENT_3D('',#14414,#11576,#11577);
#10242=AXIS2_PLACEMENT_3D('',#14418,#11580,#11581);
#10243=AXIS2_PLACEMENT_3D('',#14420,#11583,#11584);
#10244=AXIS2_PLACEMENT_3D('',#14421,#11585,#11586);
#10245=AXIS2_PLACEMENT_3D('',#14425,#11589,#11590);
#10246=AXIS2_PLACEMENT_3D('',#14429,#11593,#11594);
#10247=AXIS2_PLACEMENT_3D('',#14433,#11597,#11598);
#10248=AXIS2_PLACEMENT_3D('',#14437,#11601,#11602);
#10249=AXIS2_PLACEMENT_3D('',#14439,#11604,#11605);
#10250=AXIS2_PLACEMENT_3D('',#14440,#11606,#11607);
#10251=AXIS2_PLACEMENT_3D('',#14443,#11610,#11611);
#10252=AXIS2_PLACEMENT_3D('',#14446,#11614,#11615);
#10253=AXIS2_PLACEMENT_3D('',#14453,#11621,#11622);
#10254=AXIS2_PLACEMENT_3D('',#14460,#11628,#11629);
#10255=AXIS2_PLACEMENT_3D('',#14461,#11630,#11631);
#10256=AXIS2_PLACEMENT_3D('',#14462,#11632,#11633);
#10257=AXIS2_PLACEMENT_3D('',#14463,#11634,#11635);
#10258=AXIS2_PLACEMENT_3D('',#14464,#11636,#11637);
#10259=AXIS2_PLACEMENT_3D('',#14465,#11638,#11639);
#10260=AXIS2_PLACEMENT_3D('',#14466,#11640,#11641);
#10261=AXIS2_PLACEMENT_3D('',#14467,#11642,#11643);
#10262=AXIS2_PLACEMENT_3D('',#14469,#11645,#11646);
#10263=AXIS2_PLACEMENT_3D('',#14470,#11647,#11648);
#10264=AXIS2_PLACEMENT_3D('',#14471,#11649,#11650);
#10265=AXIS2_PLACEMENT_3D('',#14472,#11651,#11652);
#10266=AXIS2_PLACEMENT_3D('',#14473,#11653,#11654);
#10267=AXIS2_PLACEMENT_3D('',#14474,#11655,#11656);
#10268=AXIS2_PLACEMENT_3D('',#14476,#11657,#11658);
#10269=AXIS2_PLACEMENT_3D('',#14479,#11660,#11661);
#10270=AXIS2_PLACEMENT_3D('',#14480,#11662,#11663);
#10271=AXIS2_PLACEMENT_3D('',#14482,#11664,#11665);
#10272=AXIS2_PLACEMENT_3D('',#14485,#11667,#11668);
#10273=AXIS2_PLACEMENT_3D('',#14486,#11669,#11670);
#10274=AXIS2_PLACEMENT_3D('',#14488,#11671,#11672);
#10275=AXIS2_PLACEMENT_3D('',#14491,#11674,#11675);
#10276=AXIS2_PLACEMENT_3D('',#14492,#11676,#11677);
#10277=AXIS2_PLACEMENT_3D('',#14494,#11678,#11679);
#10278=AXIS2_PLACEMENT_3D('',#14497,#11681,#11682);
#10279=AXIS2_PLACEMENT_3D('',#14498,#11683,#11684);
#10280=AXIS2_PLACEMENT_3D('',#14500,#11685,#11686);
#10281=AXIS2_PLACEMENT_3D('',#14503,#11688,#11689);
#10282=AXIS2_PLACEMENT_3D('',#14504,#11690,#11691);
#10283=AXIS2_PLACEMENT_3D('',#14513,#11696,#11697);
#10284=AXIS2_PLACEMENT_3D('',#14522,#11702,#11703);
#10285=AXIS2_PLACEMENT_3D('',#14528,#11707,#11708);
#10286=AXIS2_PLACEMENT_3D('',#14534,#11712,#11713);
#10287=AXIS2_PLACEMENT_3D('',#14540,#11717,#11718);
#10288=AXIS2_PLACEMENT_3D('',#14546,#11722,#11723);
#10289=AXIS2_PLACEMENT_3D('',#14549,#11726,#11727);
#10290=AXIS2_PLACEMENT_3D('',#14555,#11731,#11732);
#10291=AXIS2_PLACEMENT_3D('',#14561,#11736,#11737);
#10292=AXIS2_PLACEMENT_3D('',#14563,#11739,#11740);
#10293=AXIS2_PLACEMENT_3D('',#14565,#11742,#11743);
#10294=AXIS2_PLACEMENT_3D('',#14566,#11744,#11745);
#10295=AXIS2_PLACEMENT_3D('',#14567,#11746,#11747);
#10296=AXIS2_PLACEMENT_3D('',#14568,#11748,#11749);
#10297=AXIS2_PLACEMENT_3D('',#14569,#11750,#11751);
#10298=AXIS2_PLACEMENT_3D('',#14570,#11752,#11753);
#10299=AXIS2_PLACEMENT_3D('',#14571,#11754,#11755);
#10300=AXIS2_PLACEMENT_3D('',#14572,#11756,#11757);
#10301=AXIS2_PLACEMENT_3D('',#14581,#11762,#11763);
#10302=AXIS2_PLACEMENT_3D('',#14587,#11767,#11768);
#10303=AXIS2_PLACEMENT_3D('',#14593,#11772,#11773);
#10304=AXIS2_PLACEMENT_3D('',#14596,#11776,#11777);
#10305=AXIS2_PLACEMENT_3D('',#14597,#11778,#11779);
#10306=AXIS2_PLACEMENT_3D('',#14598,#11780,#11781);
#10307=AXIS2_PLACEMENT_3D('',#14599,#11782,#11783);
#10308=AXIS2_PLACEMENT_3D('',#14608,#11788,#11789);
#10309=AXIS2_PLACEMENT_3D('',#14614,#11793,#11794);
#10310=AXIS2_PLACEMENT_3D('',#14620,#11798,#11799);
#10311=AXIS2_PLACEMENT_3D('',#14623,#11802,#11803);
#10312=AXIS2_PLACEMENT_3D('',#14624,#11804,#11805);
#10313=AXIS2_PLACEMENT_3D('',#14625,#11806,#11807);
#10314=AXIS2_PLACEMENT_3D('',#14626,#11808,#11809);
#10315=AXIS2_PLACEMENT_3D('',#14628,#11810,#11811);
#10316=AXIS2_PLACEMENT_3D('',#14631,#11813,#11814);
#10317=AXIS2_PLACEMENT_3D('',#14632,#11815,#11816);
#10318=AXIS2_PLACEMENT_3D('',#14634,#11817,#11818);
#10319=AXIS2_PLACEMENT_3D('',#14637,#11820,#11821);
#10320=AXIS2_PLACEMENT_3D('',#14638,#11822,#11823);
#10321=AXIS2_PLACEMENT_3D('',#14640,#11824,#11825);
#10322=AXIS2_PLACEMENT_3D('',#14643,#11827,#11828);
#10323=AXIS2_PLACEMENT_3D('',#14644,#11829,#11830);
#10324=AXIS2_PLACEMENT_3D('',#14646,#11831,#11832);
#10325=AXIS2_PLACEMENT_3D('',#14649,#11834,#11835);
#10326=AXIS2_PLACEMENT_3D('',#14650,#11836,#11837);
#10327=AXIS2_PLACEMENT_3D('',#14659,#11842,#11843);
#10328=AXIS2_PLACEMENT_3D('',#14665,#11847,#11848);
#10329=AXIS2_PLACEMENT_3D('',#14671,#11852,#11853);
#10330=AXIS2_PLACEMENT_3D('',#14674,#11856,#11857);
#10331=AXIS2_PLACEMENT_3D('',#14675,#11858,#11859);
#10332=AXIS2_PLACEMENT_3D('',#14676,#11860,#11861);
#10333=AXIS2_PLACEMENT_3D('',#14677,#11862,#11863);
#10334=AXIS2_PLACEMENT_3D('',#14678,#11864,#11865);
#10335=AXIS2_PLACEMENT_3D('',#14679,#11866,#11867);
#10336=AXIS2_PLACEMENT_3D('',#14681,#11868,#11869);
#10337=AXIS2_PLACEMENT_3D('',#14684,#11871,#11872);
#10338=AXIS2_PLACEMENT_3D('',#14685,#11873,#11874);
#10339=AXIS2_PLACEMENT_3D('',#14687,#11875,#11876);
#10340=AXIS2_PLACEMENT_3D('',#14690,#11878,#11879);
#10341=AXIS2_PLACEMENT_3D('',#14691,#11880,#11881);
#10342=AXIS2_PLACEMENT_3D('',#14693,#11882,#11883);
#10343=AXIS2_PLACEMENT_3D('',#14696,#11885,#11886);
#10344=AXIS2_PLACEMENT_3D('',#14697,#11887,#11888);
#10345=AXIS2_PLACEMENT_3D('',#14699,#11889,#11890);
#10346=AXIS2_PLACEMENT_3D('',#14702,#11892,#11893);
#10347=AXIS2_PLACEMENT_3D('',#14703,#11894,#11895);
#10348=AXIS2_PLACEMENT_3D('',#14705,#11896,#11897);
#10349=AXIS2_PLACEMENT_3D('',#14708,#11899,#11900);
#10350=AXIS2_PLACEMENT_3D('',#14709,#11901,#11902);
#10351=AXIS2_PLACEMENT_3D('',#14710,#11903,#11904);
#10352=AXIS2_PLACEMENT_3D('',#14711,#11905,#11906);
#10353=AXIS2_PLACEMENT_3D('',#14712,#11907,#11908);
#10354=AXIS2_PLACEMENT_3D('',#14713,#11909,#11910);
#10355=AXIS2_PLACEMENT_3D('',#14714,#11911,#11912);
#10356=AXIS2_PLACEMENT_3D('',#14715,#11913,#11914);
#10357=AXIS2_PLACEMENT_3D('',#14716,#11915,#11916);
#10358=AXIS2_PLACEMENT_3D('',#14718,#11917,#11918);
#10359=AXIS2_PLACEMENT_3D('',#14721,#11920,#11921);
#10360=AXIS2_PLACEMENT_3D('',#14722,#11922,#11923);
#10361=AXIS2_PLACEMENT_3D('',#14724,#11924,#11925);
#10362=AXIS2_PLACEMENT_3D('',#14727,#11927,#11928);
#10363=AXIS2_PLACEMENT_3D('',#14728,#11929,#11930);
#10364=AXIS2_PLACEMENT_3D('',#14730,#11931,#11932);
#10365=AXIS2_PLACEMENT_3D('',#14733,#11934,#11935);
#10366=AXIS2_PLACEMENT_3D('',#14734,#11936,#11937);
#10367=AXIS2_PLACEMENT_3D('',#14736,#11938,#11939);
#10368=AXIS2_PLACEMENT_3D('',#14739,#11941,#11942);
#10369=AXIS2_PLACEMENT_3D('',#14740,#11943,#11944);
#10370=AXIS2_PLACEMENT_3D('',#14742,#11945,#11946);
#10371=AXIS2_PLACEMENT_3D('',#14745,#11948,#11949);
#10372=AXIS2_PLACEMENT_3D('',#14746,#11950,#11951);
#10373=AXIS2_PLACEMENT_3D('',#14747,#11952,#11953);
#10374=AXIS2_PLACEMENT_3D('',#14748,#11954,#11955);
#10375=AXIS2_PLACEMENT_3D('',#14749,#11956,#11957);
#10376=AXIS2_PLACEMENT_3D('',#14750,#11958,#11959);
#10377=AXIS2_PLACEMENT_3D('',#14751,#11960,#11961);
#10378=AXIS2_PLACEMENT_3D('',#14752,#11962,#11963);
#10379=AXIS2_PLACEMENT_3D('',#14753,#11964,#11965);
#10380=AXIS2_PLACEMENT_3D('',#14755,#11966,#11967);
#10381=AXIS2_PLACEMENT_3D('',#14796,#11969,#11970);
#10382=AXIS2_PLACEMENT_3D('',#14819,#11972,#11973);
#10383=AXIS2_PLACEMENT_3D('',#14839,#11974,#11975);
#10384=AXIS2_PLACEMENT_3D('',#14841,#11976,#11977);
#10385=AXIS2_PLACEMENT_3D('',#14844,#11979,#11980);
#10386=AXIS2_PLACEMENT_3D('',#14845,#11981,#11982);
#10387=AXIS2_PLACEMENT_3D('',#14847,#11983,#11984);
#10388=AXIS2_PLACEMENT_3D('',#14850,#11986,#11987);
#10389=AXIS2_PLACEMENT_3D('',#14851,#11988,#11989);
#10390=AXIS2_PLACEMENT_3D('',#14854,#11990,#11991);
#10391=AXIS2_PLACEMENT_3D('',#14858,#11993,#11994);
#10392=AXIS2_PLACEMENT_3D('',#14862,#11996,#11997);
#10393=AXIS2_PLACEMENT_3D('',#14866,#12000,#12001);
#10394=AXIS2_PLACEMENT_3D('',#14868,#12002,#12003);
#10395=AXIS2_PLACEMENT_3D('',#14872,#12005,#12006);
#10396=AXIS2_PLACEMENT_3D('',#14874,#12008,#12009);
#10397=AXIS2_PLACEMENT_3D('',#14876,#12011,#12012);
#10398=AXIS2_PLACEMENT_3D('',#14878,#12014,#12015);
#10399=AXIS2_PLACEMENT_3D('',#14879,#12016,#12017);
#10400=AXIS2_PLACEMENT_3D('',#14880,#12018,#12019);
#10401=AXIS2_PLACEMENT_3D('',#14881,#12020,#12021);
#10402=AXIS2_PLACEMENT_3D('',#14883,#12023,#12024);
#10403=AXIS2_PLACEMENT_3D('',#14885,#12026,#12027);
#10404=AXIS2_PLACEMENT_3D('',#14886,#12028,#12029);
#10405=AXIS2_PLACEMENT_3D('',#14887,#12030,#12031);
#10406=AXIS2_PLACEMENT_3D('',#14889,#12032,#12033);
#10407=AXIS2_PLACEMENT_3D('',#14892,#12035,#12036);
#10408=AXIS2_PLACEMENT_3D('',#14893,#12037,#12038);
#10409=AXIS2_PLACEMENT_3D('',#14902,#12043,#12044);
#10410=AXIS2_PLACEMENT_3D('',#14911,#12049,#12050);
#10411=AXIS2_PLACEMENT_3D('',#14914,#12053,#12054);
#10412=AXIS2_PLACEMENT_3D('',#14916,#12056,#12057);
#10413=AXIS2_PLACEMENT_3D('',#14918,#12059,#12060);
#10414=AXIS2_PLACEMENT_3D('',#14919,#12061,#12062);
#10415=AXIS2_PLACEMENT_3D('',#14920,#12063,#12064);
#10416=AXIS2_PLACEMENT_3D('',#14922,#12065,#12066);
#10417=AXIS2_PLACEMENT_3D('',#14925,#12068,#12069);
#10418=AXIS2_PLACEMENT_3D('',#14926,#12070,#12071);
#10419=AXIS2_PLACEMENT_3D('',#14935,#12076,#12077);
#10420=AXIS2_PLACEMENT_3D('',#14944,#12082,#12083);
#10421=AXIS2_PLACEMENT_3D('',#14947,#12086,#12087);
#10422=AXIS2_PLACEMENT_3D('',#14949,#12089,#12090);
#10423=AXIS2_PLACEMENT_3D('',#14951,#12092,#12093);
#10424=AXIS2_PLACEMENT_3D('',#14952,#12094,#12095);
#10425=AXIS2_PLACEMENT_3D('',#14953,#12096,#12097);
#10426=AXIS2_PLACEMENT_3D('',#14955,#12098,#12099);
#10427=AXIS2_PLACEMENT_3D('',#14958,#12101,#12102);
#10428=AXIS2_PLACEMENT_3D('',#14959,#12103,#12104);
#10429=AXIS2_PLACEMENT_3D('',#14961,#12105,#12106);
#10430=AXIS2_PLACEMENT_3D('',#14981,#12107,#12108);
#10431=AXIS2_PLACEMENT_3D('',#15001,#12109,#12110);
#10432=AXIS2_PLACEMENT_3D('',#15003,#12111,#12112);
#10433=AXIS2_PLACEMENT_3D('',#15006,#12114,#12115);
#10434=AXIS2_PLACEMENT_3D('',#15007,#12116,#12117);
#10435=AXIS2_PLACEMENT_3D('',#15009,#12118,#12119);
#10436=AXIS2_PLACEMENT_3D('',#15011,#12121,#12122);
#10437=AXIS2_PLACEMENT_3D('',#15012,#12123,#12124);
#10438=AXIS2_PLACEMENT_3D('',#15013,#12125,#12126);
#10439=AXIS2_PLACEMENT_3D('',#15014,#12127,#12128);
#10440=AXIS2_PLACEMENT_3D('',#15015,#12129,#12130);
#10441=AXIS2_PLACEMENT_3D('',#15016,#12131,#12132);
#10442=AXIS2_PLACEMENT_3D('',#15018,#12133,#12134);
#10443=AXIS2_PLACEMENT_3D('',#15021,#12136,#12137);
#10444=AXIS2_PLACEMENT_3D('',#15022,#12138,#12139);
#10445=AXIS2_PLACEMENT_3D('',#15023,#12140,#12141);
#10446=AXIS2_PLACEMENT_3D('',#15024,#12142,#12143);
#10447=AXIS2_PLACEMENT_3D('',#15025,#12144,#12145);
#10448=AXIS2_PLACEMENT_3D('',#15027,#12146,#12147);
#10449=AXIS2_PLACEMENT_3D('',#15030,#12149,#12150);
#10450=AXIS2_PLACEMENT_3D('',#15031,#12151,#12152);
#10451=AXIS2_PLACEMENT_3D('',#15033,#12153,#12154);
#10452=AXIS2_PLACEMENT_3D('',#15036,#12156,#12157);
#10453=AXIS2_PLACEMENT_3D('',#15037,#12158,#12159);
#10454=AXIS2_PLACEMENT_3D('',#15039,#12160,#12161);
#10455=AXIS2_PLACEMENT_3D('',#15042,#12163,#12164);
#10456=AXIS2_PLACEMENT_3D('',#15043,#12165,#12166);
#10457=AXIS2_PLACEMENT_3D('',#15045,#12167,#12168);
#10458=AXIS2_PLACEMENT_3D('',#15048,#12170,#12171);
#10459=AXIS2_PLACEMENT_3D('',#15049,#12172,#12173);
#10460=AXIS2_PLACEMENT_3D('',#15058,#12178,#12179);
#10461=AXIS2_PLACEMENT_3D('',#15064,#12183,#12184);
#10462=AXIS2_PLACEMENT_3D('',#15070,#12188,#12189);
#10463=AXIS2_PLACEMENT_3D('',#15073,#12192,#12193);
#10464=AXIS2_PLACEMENT_3D('',#15074,#12194,#12195);
#10465=AXIS2_PLACEMENT_3D('',#15075,#12196,#12197);
#10466=AXIS2_PLACEMENT_3D('',#15076,#12198,#12199);
#10467=AXIS2_PLACEMENT_3D('',#15077,#12200,#12201);
#10468=AXIS2_PLACEMENT_3D('',#15078,#12202,#12203);
#10469=AXIS2_PLACEMENT_3D('',#15080,#12204,#12205);
#10470=AXIS2_PLACEMENT_3D('',#15083,#12207,#12208);
#10471=AXIS2_PLACEMENT_3D('',#15084,#12209,#12210);
#10472=AXIS2_PLACEMENT_3D('',#15086,#12211,#12212);
#10473=AXIS2_PLACEMENT_3D('',#15089,#12214,#12215);
#10474=AXIS2_PLACEMENT_3D('',#15090,#12216,#12217);
#10475=AXIS2_PLACEMENT_3D('',#15092,#12218,#12219);
#10476=AXIS2_PLACEMENT_3D('',#15095,#12221,#12222);
#10477=AXIS2_PLACEMENT_3D('',#15096,#12223,#12224);
#10478=AXIS2_PLACEMENT_3D('',#15113,#12233,#12234);
#10479=AXIS2_PLACEMENT_3D('',#15130,#12243,#12244);
#10480=AXIS2_PLACEMENT_3D('',#15133,#12247,#12248);
#10481=AXIS2_PLACEMENT_3D('',#15135,#12250,#12251);
#10482=AXIS2_PLACEMENT_3D('',#15137,#12253,#12254);
#10483=AXIS2_PLACEMENT_3D('',#15139,#12256,#12257);
#10484=AXIS2_PLACEMENT_3D('',#15141,#12259,#12260);
#10485=AXIS2_PLACEMENT_3D('',#15143,#12262,#12263);
#10486=AXIS2_PLACEMENT_3D('',#15145,#12265,#12266);
#10487=AXIS2_PLACEMENT_3D('',#15146,#12267,#12268);
#10488=AXIS2_PLACEMENT_3D('',#15147,#12269,#12270);
#10489=AXIS2_PLACEMENT_3D('',#15149,#12271,#12272);
#10490=AXIS2_PLACEMENT_3D('',#15152,#12274,#12275);
#10491=AXIS2_PLACEMENT_3D('',#15153,#12276,#12277);
#10492=AXIS2_PLACEMENT_3D('',#15155,#12278,#12279);
#10493=AXIS2_PLACEMENT_3D('',#15159,#12281,#12282);
#10494=AXIS2_PLACEMENT_3D('',#15163,#12284,#12285);
#10495=AXIS2_PLACEMENT_3D('',#15166,#12287,#12288);
#10496=AXIS2_PLACEMENT_3D('',#15168,#12289,#12290);
#10497=AXIS2_PLACEMENT_3D('',#15171,#12292,#12293);
#10498=AXIS2_PLACEMENT_3D('',#15174,#12294,#12295);
#10499=AXIS2_PLACEMENT_3D('',#15178,#12297,#12298);
#10500=AXIS2_PLACEMENT_3D('',#15184,#12301,#12302);
#10501=AXIS2_PLACEMENT_3D('',#15187,#12304,#12305);
#10502=AXIS2_PLACEMENT_3D('',#15192,#12307,#12308);
#10503=AXIS2_PLACEMENT_3D('',#15195,#12310,#12311);
#10504=AXIS2_PLACEMENT_3D('',#15200,#12313,#12314);
#10505=AXIS2_PLACEMENT_3D('',#15203,#12316,#12317);
#10506=AXIS2_PLACEMENT_3D('',#15208,#12319,#12320);
#10507=AXIS2_PLACEMENT_3D('',#15211,#12322,#12323);
#10508=AXIS2_PLACEMENT_3D('',#15216,#12325,#12326);
#10509=AXIS2_PLACEMENT_3D('',#15219,#12328,#12329);
#10510=AXIS2_PLACEMENT_3D('',#15224,#12331,#12332);
#10511=AXIS2_PLACEMENT_3D('',#15227,#12334,#12335);
#10512=AXIS2_PLACEMENT_3D('',#15232,#12337,#12338);
#10513=AXIS2_PLACEMENT_3D('',#15235,#12340,#12341);
#10514=AXIS2_PLACEMENT_3D('',#15240,#12343,#12344);
#10515=AXIS2_PLACEMENT_3D('',#15243,#12346,#12347);
#10516=AXIS2_PLACEMENT_3D('',#15248,#12349,#12350);
#10517=AXIS2_PLACEMENT_3D('',#15251,#12352,#12353);
#10518=AXIS2_PLACEMENT_3D('',#15256,#12355,#12356);
#10519=AXIS2_PLACEMENT_3D('',#15259,#12358,#12359);
#10520=AXIS2_PLACEMENT_3D('',#15264,#12361,#12362);
#10521=AXIS2_PLACEMENT_3D('',#15267,#12364,#12365);
#10522=AXIS2_PLACEMENT_3D('',#15272,#12367,#12368);
#10523=AXIS2_PLACEMENT_3D('',#15275,#12370,#12371);
#10524=AXIS2_PLACEMENT_3D('',#15280,#12373,#12374);
#10525=AXIS2_PLACEMENT_3D('',#15283,#12376,#12377);
#10526=AXIS2_PLACEMENT_3D('',#15288,#12379,#12380);
#10527=AXIS2_PLACEMENT_3D('',#15291,#12382,#12383);
#10528=AXIS2_PLACEMENT_3D('',#15296,#12385,#12386);
#10529=AXIS2_PLACEMENT_3D('',#15299,#12388,#12389);
#10530=AXIS2_PLACEMENT_3D('',#15304,#12391,#12392);
#10531=AXIS2_PLACEMENT_3D('',#15307,#12394,#12395);
#10532=AXIS2_PLACEMENT_3D('',#15312,#12397,#12398);
#10533=AXIS2_PLACEMENT_3D('',#15315,#12400,#12401);
#10534=AXIS2_PLACEMENT_3D('',#15320,#12403,#12404);
#10535=AXIS2_PLACEMENT_3D('',#15323,#12406,#12407);
#10536=AXIS2_PLACEMENT_3D('',#15328,#12409,#12410);
#10537=AXIS2_PLACEMENT_3D('',#15331,#12412,#12413);
#10538=AXIS2_PLACEMENT_3D('',#15336,#12415,#12416);
#10539=AXIS2_PLACEMENT_3D('',#15339,#12418,#12419);
#10540=AXIS2_PLACEMENT_3D('',#15344,#12421,#12422);
#10541=AXIS2_PLACEMENT_3D('',#15347,#12424,#12425);
#10542=AXIS2_PLACEMENT_3D('',#15352,#12427,#12428);
#10543=AXIS2_PLACEMENT_3D('',#15355,#12430,#12431);
#10544=AXIS2_PLACEMENT_3D('',#15360,#12433,#12434);
#10545=AXIS2_PLACEMENT_3D('',#15363,#12436,#12437);
#10546=AXIS2_PLACEMENT_3D('',#15368,#12439,#12440);
#10547=AXIS2_PLACEMENT_3D('',#15371,#12442,#12443);
#10548=AXIS2_PLACEMENT_3D('',#15376,#12445,#12446);
#10549=AXIS2_PLACEMENT_3D('',#15379,#12448,#12449);
#10550=AXIS2_PLACEMENT_3D('',#15384,#12451,#12452);
#10551=AXIS2_PLACEMENT_3D('',#15387,#12454,#12455);
#10552=AXIS2_PLACEMENT_3D('',#15392,#12457,#12458);
#10553=AXIS2_PLACEMENT_3D('',#15395,#12460,#12461);
#10554=AXIS2_PLACEMENT_3D('',#15400,#12463,#12464);
#10555=AXIS2_PLACEMENT_3D('',#15403,#12466,#12467);
#10556=AXIS2_PLACEMENT_3D('',#15408,#12469,#12470);
#10557=AXIS2_PLACEMENT_3D('',#15411,#12472,#12473);
#10558=AXIS2_PLACEMENT_3D('',#15416,#12475,#12476);
#10559=AXIS2_PLACEMENT_3D('',#15419,#12478,#12479);
#10560=AXIS2_PLACEMENT_3D('',#15424,#12481,#12482);
#10561=AXIS2_PLACEMENT_3D('',#15427,#12484,#12485);
#10562=AXIS2_PLACEMENT_3D('',#15432,#12487,#12488);
#10563=AXIS2_PLACEMENT_3D('',#15435,#12490,#12491);
#10564=AXIS2_PLACEMENT_3D('',#15440,#12493,#12494);
#10565=AXIS2_PLACEMENT_3D('',#15443,#12496,#12497);
#10566=AXIS2_PLACEMENT_3D('',#15448,#12499,#12500);
#10567=AXIS2_PLACEMENT_3D('',#15451,#12502,#12503);
#10568=AXIS2_PLACEMENT_3D('',#15456,#12505,#12506);
#10569=AXIS2_PLACEMENT_3D('',#15459,#12508,#12509);
#10570=AXIS2_PLACEMENT_3D('',#15464,#12511,#12512);
#10571=AXIS2_PLACEMENT_3D('',#15467,#12514,#12515);
#10572=AXIS2_PLACEMENT_3D('',#15472,#12517,#12518);
#10573=AXIS2_PLACEMENT_3D('',#15475,#12520,#12521);
#10574=AXIS2_PLACEMENT_3D('',#15480,#12523,#12524);
#10575=AXIS2_PLACEMENT_3D('',#15483,#12526,#12527);
#10576=AXIS2_PLACEMENT_3D('',#15484,#12528,#12529);
#10577=AXIS2_PLACEMENT_3D('',#15485,#12530,#12531);
#10578=AXIS2_PLACEMENT_3D('',#15486,#12532,#12533);
#10579=AXIS2_PLACEMENT_3D('',#15492,#12537,#12538);
#10580=AXIS2_PLACEMENT_3D('',#15498,#12542,#12543);
#10581=AXIS2_PLACEMENT_3D('',#15500,#12545,#12546);
#10582=AXIS2_PLACEMENT_3D('',#15502,#12548,#12549);
#10583=AXIS2_PLACEMENT_3D('',#15503,#12550,#12551);
#10584=AXIS2_PLACEMENT_3D('',#15509,#12555,#12556);
#10585=AXIS2_PLACEMENT_3D('',#15515,#12560,#12561);
#10586=AXIS2_PLACEMENT_3D('',#15517,#12563,#12564);
#10587=AXIS2_PLACEMENT_3D('',#15519,#12566,#12567);
#10588=AXIS2_PLACEMENT_3D('',#15520,#12568,#12569);
#10589=AXIS2_PLACEMENT_3D('',#15526,#12573,#12574);
#10590=AXIS2_PLACEMENT_3D('',#15532,#12578,#12579);
#10591=AXIS2_PLACEMENT_3D('',#15534,#12581,#12582);
#10592=AXIS2_PLACEMENT_3D('',#15536,#12584,#12585);
#10593=AXIS2_PLACEMENT_3D('',#15537,#12586,#12587);
#10594=AXIS2_PLACEMENT_3D('',#15543,#12591,#12592);
#10595=AXIS2_PLACEMENT_3D('',#15549,#12596,#12597);
#10596=AXIS2_PLACEMENT_3D('',#15551,#12599,#12600);
#10597=AXIS2_PLACEMENT_3D('',#15553,#12602,#12603);
#10598=AXIS2_PLACEMENT_3D('',#15554,#12604,#12605);
#10599=AXIS2_PLACEMENT_3D('',#15560,#12609,#12610);
#10600=AXIS2_PLACEMENT_3D('',#15566,#12614,#12615);
#10601=AXIS2_PLACEMENT_3D('',#15568,#12617,#12618);
#10602=AXIS2_PLACEMENT_3D('',#15570,#12620,#12621);
#10603=AXIS2_PLACEMENT_3D('',#15571,#12622,#12623);
#10604=AXIS2_PLACEMENT_3D('',#15577,#12627,#12628);
#10605=AXIS2_PLACEMENT_3D('',#15583,#12632,#12633);
#10606=AXIS2_PLACEMENT_3D('',#15585,#12635,#12636);
#10607=AXIS2_PLACEMENT_3D('',#15587,#12638,#12639);
#10608=AXIS2_PLACEMENT_3D('',#15588,#12640,#12641);
#10609=AXIS2_PLACEMENT_3D('',#15594,#12645,#12646);
#10610=AXIS2_PLACEMENT_3D('',#15600,#12650,#12651);
#10611=AXIS2_PLACEMENT_3D('',#15602,#12653,#12654);
#10612=AXIS2_PLACEMENT_3D('',#15604,#12656,#12657);
#10613=AXIS2_PLACEMENT_3D('',#15605,#12658,#12659);
#10614=AXIS2_PLACEMENT_3D('',#15611,#12663,#12664);
#10615=AXIS2_PLACEMENT_3D('',#15617,#12668,#12669);
#10616=AXIS2_PLACEMENT_3D('',#15619,#12671,#12672);
#10617=AXIS2_PLACEMENT_3D('',#15621,#12674,#12675);
#10618=AXIS2_PLACEMENT_3D('',#15622,#12676,#12677);
#10619=AXIS2_PLACEMENT_3D('',#15628,#12681,#12682);
#10620=AXIS2_PLACEMENT_3D('',#15634,#12686,#12687);
#10621=AXIS2_PLACEMENT_3D('',#15636,#12689,#12690);
#10622=AXIS2_PLACEMENT_3D('',#15638,#12692,#12693);
#10623=AXIS2_PLACEMENT_3D('',#15639,#12694,#12695);
#10624=AXIS2_PLACEMENT_3D('',#15645,#12699,#12700);
#10625=AXIS2_PLACEMENT_3D('',#15651,#12704,#12705);
#10626=AXIS2_PLACEMENT_3D('',#15653,#12707,#12708);
#10627=AXIS2_PLACEMENT_3D('',#15655,#12710,#12711);
#10628=AXIS2_PLACEMENT_3D('',#15656,#12712,#12713);
#10629=AXIS2_PLACEMENT_3D('',#15662,#12717,#12718);
#10630=AXIS2_PLACEMENT_3D('',#15668,#12722,#12723);
#10631=AXIS2_PLACEMENT_3D('',#15670,#12725,#12726);
#10632=AXIS2_PLACEMENT_3D('',#15672,#12728,#12729);
#10633=AXIS2_PLACEMENT_3D('',#15673,#12730,#12731);
#10634=AXIS2_PLACEMENT_3D('',#15679,#12735,#12736);
#10635=AXIS2_PLACEMENT_3D('',#15685,#12740,#12741);
#10636=AXIS2_PLACEMENT_3D('',#15687,#12743,#12744);
#10637=AXIS2_PLACEMENT_3D('',#15689,#12746,#12747);
#10638=AXIS2_PLACEMENT_3D('',#15690,#12748,#12749);
#10639=AXIS2_PLACEMENT_3D('',#15696,#12753,#12754);
#10640=AXIS2_PLACEMENT_3D('',#15702,#12758,#12759);
#10641=AXIS2_PLACEMENT_3D('',#15704,#12761,#12762);
#10642=AXIS2_PLACEMENT_3D('',#15706,#12764,#12765);
#10643=AXIS2_PLACEMENT_3D('',#15707,#12766,#12767);
#10644=AXIS2_PLACEMENT_3D('',#15713,#12771,#12772);
#10645=AXIS2_PLACEMENT_3D('',#15719,#12776,#12777);
#10646=AXIS2_PLACEMENT_3D('',#15721,#12779,#12780);
#10647=AXIS2_PLACEMENT_3D('',#15723,#12782,#12783);
#10648=AXIS2_PLACEMENT_3D('',#15724,#12784,#12785);
#10649=AXIS2_PLACEMENT_3D('',#15730,#12789,#12790);
#10650=AXIS2_PLACEMENT_3D('',#15736,#12794,#12795);
#10651=AXIS2_PLACEMENT_3D('',#15738,#12797,#12798);
#10652=AXIS2_PLACEMENT_3D('',#15740,#12800,#12801);
#10653=AXIS2_PLACEMENT_3D('',#15741,#12802,#12803);
#10654=AXIS2_PLACEMENT_3D('',#15747,#12807,#12808);
#10655=AXIS2_PLACEMENT_3D('',#15753,#12812,#12813);
#10656=AXIS2_PLACEMENT_3D('',#15755,#12815,#12816);
#10657=AXIS2_PLACEMENT_3D('',#15757,#12818,#12819);
#10658=AXIS2_PLACEMENT_3D('',#15758,#12820,#12821);
#10659=AXIS2_PLACEMENT_3D('',#15764,#12825,#12826);
#10660=AXIS2_PLACEMENT_3D('',#15770,#12830,#12831);
#10661=AXIS2_PLACEMENT_3D('',#15772,#12833,#12834);
#10662=AXIS2_PLACEMENT_3D('',#15774,#12836,#12837);
#10663=AXIS2_PLACEMENT_3D('',#15775,#12838,#12839);
#10664=AXIS2_PLACEMENT_3D('',#15781,#12843,#12844);
#10665=AXIS2_PLACEMENT_3D('',#15787,#12848,#12849);
#10666=AXIS2_PLACEMENT_3D('',#15789,#12851,#12852);
#10667=AXIS2_PLACEMENT_3D('',#15791,#12854,#12855);
#10668=AXIS2_PLACEMENT_3D('',#15792,#12856,#12857);
#10669=AXIS2_PLACEMENT_3D('',#15798,#12861,#12862);
#10670=AXIS2_PLACEMENT_3D('',#15804,#12866,#12867);
#10671=AXIS2_PLACEMENT_3D('',#15806,#12869,#12870);
#10672=AXIS2_PLACEMENT_3D('',#15808,#12872,#12873);
#10673=AXIS2_PLACEMENT_3D('',#15809,#12874,#12875);
#10674=AXIS2_PLACEMENT_3D('',#15815,#12879,#12880);
#10675=AXIS2_PLACEMENT_3D('',#15821,#12884,#12885);
#10676=AXIS2_PLACEMENT_3D('',#15823,#12887,#12888);
#10677=AXIS2_PLACEMENT_3D('',#15825,#12890,#12891);
#10678=AXIS2_PLACEMENT_3D('',#15826,#12892,#12893);
#10679=AXIS2_PLACEMENT_3D('',#15832,#12897,#12898);
#10680=AXIS2_PLACEMENT_3D('',#15838,#12902,#12903);
#10681=AXIS2_PLACEMENT_3D('',#15840,#12905,#12906);
#10682=AXIS2_PLACEMENT_3D('',#15842,#12908,#12909);
#10683=AXIS2_PLACEMENT_3D('',#15843,#12910,#12911);
#10684=AXIS2_PLACEMENT_3D('',#15849,#12915,#12916);
#10685=AXIS2_PLACEMENT_3D('',#15855,#12920,#12921);
#10686=AXIS2_PLACEMENT_3D('',#15857,#12923,#12924);
#10687=AXIS2_PLACEMENT_3D('',#15859,#12926,#12927);
#10688=AXIS2_PLACEMENT_3D('',#15860,#12928,#12929);
#10689=AXIS2_PLACEMENT_3D('',#15866,#12933,#12934);
#10690=AXIS2_PLACEMENT_3D('',#15872,#12938,#12939);
#10691=AXIS2_PLACEMENT_3D('',#15874,#12941,#12942);
#10692=AXIS2_PLACEMENT_3D('',#15876,#12944,#12945);
#10693=AXIS2_PLACEMENT_3D('',#15877,#12946,#12947);
#10694=AXIS2_PLACEMENT_3D('',#15883,#12951,#12952);
#10695=AXIS2_PLACEMENT_3D('',#15889,#12956,#12957);
#10696=AXIS2_PLACEMENT_3D('',#15891,#12959,#12960);
#10697=AXIS2_PLACEMENT_3D('',#15893,#12962,#12963);
#10698=AXIS2_PLACEMENT_3D('',#15894,#12964,#12965);
#10699=AXIS2_PLACEMENT_3D('',#15900,#12969,#12970);
#10700=AXIS2_PLACEMENT_3D('',#15906,#12974,#12975);
#10701=AXIS2_PLACEMENT_3D('',#15908,#12977,#12978);
#10702=AXIS2_PLACEMENT_3D('',#15910,#12980,#12981);
#10703=AXIS2_PLACEMENT_3D('',#15911,#12982,#12983);
#10704=AXIS2_PLACEMENT_3D('',#15917,#12987,#12988);
#10705=AXIS2_PLACEMENT_3D('',#15923,#12992,#12993);
#10706=AXIS2_PLACEMENT_3D('',#15925,#12995,#12996);
#10707=AXIS2_PLACEMENT_3D('',#15927,#12998,#12999);
#10708=AXIS2_PLACEMENT_3D('',#15928,#13000,#13001);
#10709=AXIS2_PLACEMENT_3D('',#15934,#13005,#13006);
#10710=AXIS2_PLACEMENT_3D('',#15940,#13010,#13011);
#10711=AXIS2_PLACEMENT_3D('',#15942,#13013,#13014);
#10712=AXIS2_PLACEMENT_3D('',#15944,#13016,#13017);
#10713=AXIS2_PLACEMENT_3D('',#15945,#13018,#13019);
#10714=AXIS2_PLACEMENT_3D('',#15951,#13023,#13024);
#10715=AXIS2_PLACEMENT_3D('',#15957,#13028,#13029);
#10716=AXIS2_PLACEMENT_3D('',#15959,#13031,#13032);
#10717=AXIS2_PLACEMENT_3D('',#15961,#13034,#13035);
#10718=AXIS2_PLACEMENT_3D('',#15962,#13036,#13037);
#10719=AXIS2_PLACEMENT_3D('',#15968,#13041,#13042);
#10720=AXIS2_PLACEMENT_3D('',#15974,#13046,#13047);
#10721=AXIS2_PLACEMENT_3D('',#15976,#13049,#13050);
#10722=AXIS2_PLACEMENT_3D('',#15978,#13052,#13053);
#10723=AXIS2_PLACEMENT_3D('',#15979,#13054,#13055);
#10724=AXIS2_PLACEMENT_3D('',#15985,#13059,#13060);
#10725=AXIS2_PLACEMENT_3D('',#15991,#13064,#13065);
#10726=AXIS2_PLACEMENT_3D('',#15993,#13067,#13068);
#10727=AXIS2_PLACEMENT_3D('',#15995,#13070,#13071);
#10728=AXIS2_PLACEMENT_3D('',#15996,#13072,#13073);
#10729=AXIS2_PLACEMENT_3D('',#16002,#13077,#13078);
#10730=AXIS2_PLACEMENT_3D('',#16008,#13082,#13083);
#10731=AXIS2_PLACEMENT_3D('',#16010,#13085,#13086);
#10732=AXIS2_PLACEMENT_3D('',#16012,#13088,#13089);
#10733=AXIS2_PLACEMENT_3D('',#16013,#13090,#13091);
#10734=AXIS2_PLACEMENT_3D('',#16019,#13095,#13096);
#10735=AXIS2_PLACEMENT_3D('',#16025,#13100,#13101);
#10736=AXIS2_PLACEMENT_3D('',#16027,#13103,#13104);
#10737=AXIS2_PLACEMENT_3D('',#16029,#13106,#13107);
#10738=AXIS2_PLACEMENT_3D('',#16030,#13108,#13109);
#10739=AXIS2_PLACEMENT_3D('',#16036,#13113,#13114);
#10740=AXIS2_PLACEMENT_3D('',#16042,#13118,#13119);
#10741=AXIS2_PLACEMENT_3D('',#16044,#13121,#13122);
#10742=AXIS2_PLACEMENT_3D('',#16046,#13124,#13125);
#10743=AXIS2_PLACEMENT_3D('',#16047,#13126,#13127);
#10744=AXIS2_PLACEMENT_3D('',#16053,#13131,#13132);
#10745=AXIS2_PLACEMENT_3D('',#16059,#13136,#13137);
#10746=AXIS2_PLACEMENT_3D('',#16061,#13139,#13140);
#10747=AXIS2_PLACEMENT_3D('',#16063,#13142,#13143);
#10748=AXIS2_PLACEMENT_3D('',#16064,#13144,#13145);
#10749=AXIS2_PLACEMENT_3D('',#16070,#13149,#13150);
#10750=AXIS2_PLACEMENT_3D('',#16076,#13154,#13155);
#10751=AXIS2_PLACEMENT_3D('',#16078,#13157,#13158);
#10752=AXIS2_PLACEMENT_3D('',#16080,#13160,#13161);
#10753=AXIS2_PLACEMENT_3D('',#16081,#13162,#13163);
#10754=AXIS2_PLACEMENT_3D('',#16087,#13167,#13168);
#10755=AXIS2_PLACEMENT_3D('',#16093,#13172,#13173);
#10756=AXIS2_PLACEMENT_3D('',#16095,#13175,#13176);
#10757=AXIS2_PLACEMENT_3D('',#16097,#13178,#13179);
#10758=AXIS2_PLACEMENT_3D('',#16098,#13180,#13181);
#10759=AXIS2_PLACEMENT_3D('',#16104,#13185,#13186);
#10760=AXIS2_PLACEMENT_3D('',#16110,#13190,#13191);
#10761=AXIS2_PLACEMENT_3D('',#16112,#13193,#13194);
#10762=AXIS2_PLACEMENT_3D('',#16114,#13196,#13197);
#10763=AXIS2_PLACEMENT_3D('',#16115,#13198,#13199);
#10764=AXIS2_PLACEMENT_3D('',#16121,#13203,#13204);
#10765=AXIS2_PLACEMENT_3D('',#16127,#13208,#13209);
#10766=AXIS2_PLACEMENT_3D('',#16129,#13211,#13212);
#10767=AXIS2_PLACEMENT_3D('',#16131,#13214,#13215);
#10768=AXIS2_PLACEMENT_3D('',#16132,#13216,#13217);
#10769=AXIS2_PLACEMENT_3D('',#16138,#13221,#13222);
#10770=AXIS2_PLACEMENT_3D('',#16144,#13226,#13227);
#10771=AXIS2_PLACEMENT_3D('',#16146,#13229,#13230);
#10772=AXIS2_PLACEMENT_3D('',#16148,#13232,#13233);
#10773=AXIS2_PLACEMENT_3D('',#16149,#13234,#13235);
#10774=AXIS2_PLACEMENT_3D('',#16155,#13239,#13240);
#10775=AXIS2_PLACEMENT_3D('',#16161,#13244,#13245);
#10776=AXIS2_PLACEMENT_3D('',#16163,#13247,#13248);
#10777=AXIS2_PLACEMENT_3D('',#16165,#13250,#13251);
#10778=AXIS2_PLACEMENT_3D('',#16166,#13252,#13253);
#10779=AXIS2_PLACEMENT_3D('',#16167,#13254,#13255);
#10780=AXIS2_PLACEMENT_3D('',#16169,#13256,#13257);
#10781=AXIS2_PLACEMENT_3D('',#16172,#13259,#13260);
#10782=AXIS2_PLACEMENT_3D('',#16173,#13261,#13262);
#10783=AXIS2_PLACEMENT_3D('',#16175,#13263,#13264);
#10784=AXIS2_PLACEMENT_3D('',#16178,#13266,#13267);
#10785=AXIS2_PLACEMENT_3D('',#16179,#13268,#13269);
#10786=AXIS2_PLACEMENT_3D('',#16208,#13284,#13285);
#10787=AXIS2_PLACEMENT_3D('',#16237,#13300,#13301);
#10788=AXIS2_PLACEMENT_3D('',#16240,#13304,#13305);
#10789=AXIS2_PLACEMENT_3D('',#16242,#13307,#13308);
#10790=AXIS2_PLACEMENT_3D('',#16244,#13310,#13311);
#10791=AXIS2_PLACEMENT_3D('',#16246,#13313,#13314);
#10792=AXIS2_PLACEMENT_3D('',#16248,#13316,#13317);
#10793=AXIS2_PLACEMENT_3D('',#16250,#13319,#13320);
#10794=AXIS2_PLACEMENT_3D('',#16252,#13322,#13323);
#10795=AXIS2_PLACEMENT_3D('',#16254,#13325,#13326);
#10796=AXIS2_PLACEMENT_3D('',#16256,#13328,#13329);
#10797=AXIS2_PLACEMENT_3D('',#16258,#13331,#13332);
#10798=AXIS2_PLACEMENT_3D('',#16260,#13334,#13335);
#10799=AXIS2_PLACEMENT_3D('',#16262,#13337,#13338);
#10800=AXIS2_PLACEMENT_3D('',#16264,#13340,#13341);
#10801=AXIS2_PLACEMENT_3D('',#16265,#13342,#13343);
#10802=AXIS2_PLACEMENT_3D('',#16266,#13344,#13345);
#10803=AXIS2_PLACEMENT_3D('',#16268,#13346,#13347);
#10804=AXIS2_PLACEMENT_3D('',#16271,#13349,#13350);
#10805=AXIS2_PLACEMENT_3D('',#16272,#13351,#13352);
#10806=AXIS2_PLACEMENT_3D('',#16275,#13353,#13354);
#10807=AXIS2_PLACEMENT_3D('',#16276,#13355,#13356);
#10808=AXIS2_PLACEMENT_3D('',#16278,#13358,#13359);
#10809=AXIS2_PLACEMENT_3D('',#16281,#13361,#13362);
#10810=AXIS2_PLACEMENT_3D('',#16282,#13363,#13364);
#10811=AXIS2_PLACEMENT_3D('',#16284,#13365,#13366);
#10812=AXIS2_PLACEMENT_3D('',#16287,#13368,#13369);
#10813=AXIS2_PLACEMENT_3D('',#16288,#13370,#13371);
#10814=AXIS2_PLACEMENT_3D('',#16289,#13372,#13373);
#10815=AXIS2_PLACEMENT_3D('',#16290,#13374,#13375);
#10816=AXIS2_PLACEMENT_3D('',#16291,#13376,#13377);
#10817=AXIS2_PLACEMENT_3D('',#16293,#13378,#13379);
#10818=AXIS2_PLACEMENT_3D('',#16296,#13381,#13382);
#10819=AXIS2_PLACEMENT_3D('',#16297,#13383,#13384);
#10820=AXIS2_PLACEMENT_3D('',#16299,#13385,#13386);
#10821=AXIS2_PLACEMENT_3D('',#16302,#13388,#13389);
#10822=AXIS2_PLACEMENT_3D('',#16303,#13390,#13391);
#10823=AXIS2_PLACEMENT_3D('',#16304,#13392,#13393);
#10824=AXIS2_PLACEMENT_3D('',#16305,#13394,#13395);
#10825=AXIS2_PLACEMENT_3D('',#16306,#13396,#13397);
#10826=AXIS2_PLACEMENT_3D('',#16307,#13398,#13399);
#10827=AXIS2_PLACEMENT_3D('',#16309,#13400,#13401);
#10828=AXIS2_PLACEMENT_3D('',#16312,#13403,#13404);
#10829=AXIS2_PLACEMENT_3D('',#16313,#13405,#13406);
#10830=AXIS2_PLACEMENT_3D('',#16326,#13413,#13414);
#10831=AXIS2_PLACEMENT_3D('',#16339,#13421,#13422);
#10832=AXIS2_PLACEMENT_3D('',#16342,#13425,#13426);
#10833=AXIS2_PLACEMENT_3D('',#16344,#13428,#13429);
#10834=AXIS2_PLACEMENT_3D('',#16346,#13431,#13432);
#10835=AXIS2_PLACEMENT_3D('',#16348,#13434,#13435);
#10836=AXIS2_PLACEMENT_3D('',#16350,#13437,#13438);
#10837=AXIS2_PLACEMENT_3D('',#16351,#13439,#13440);
#10838=AXIS2_PLACEMENT_3D('',#16352,#13441,#13442);
#10839=AXIS2_PLACEMENT_3D('',#16354,#13443,#13444);
#10840=AXIS2_PLACEMENT_3D('',#16357,#13446,#13447);
#10841=AXIS2_PLACEMENT_3D('',#16358,#13448,#13449);
#10842=AXIS2_PLACEMENT_3D('',#16360,#13450,#13451);
#10843=AXIS2_PLACEMENT_3D('',#16363,#13453,#13454);
#10844=AXIS2_PLACEMENT_3D('',#16364,#13455,#13456);
#10845=AXIS2_PLACEMENT_3D('',#16377,#13463,#13464);
#10846=AXIS2_PLACEMENT_3D('',#16378,#13465,#13466);
#10847=AXIS2_PLACEMENT_3D('',#16379,#13467,#13468);
#10848=AXIS2_PLACEMENT_3D('',#16385,#13472,#13473);
#10849=AXIS2_PLACEMENT_3D('',#16389,#13476,#13477);
#10850=AXIS2_PLACEMENT_3D('',#16393,#13480,#13481);
#10851=AXIS2_PLACEMENT_3D('',#16397,#13484,#13485);
#10852=AXIS2_PLACEMENT_3D('',#16401,#13488,#13489);
#10853=AXIS2_PLACEMENT_3D('',#16403,#13491,#13492);
#10854=AXIS2_PLACEMENT_3D('',#16404,#13493,#13494);
#10855=AXIS2_PLACEMENT_3D('',#16405,#13495,#13496);
#10856=AXIS2_PLACEMENT_3D('',#16407,#13497,#13498);
#10857=AXIS2_PLACEMENT_3D('',#16410,#13500,#13501);
#10858=AXIS2_PLACEMENT_3D('',#16411,#13502,#13503);
#10859=AXIS2_PLACEMENT_3D('',#16420,#13508,#13509);
#10860=AXIS2_PLACEMENT_3D('',#16426,#13513,#13514);
#10861=AXIS2_PLACEMENT_3D('',#16432,#13518,#13519);
#10862=AXIS2_PLACEMENT_3D('',#16438,#13523,#13524);
#10863=AXIS2_PLACEMENT_3D('',#16444,#13528,#13529);
#10864=AXIS2_PLACEMENT_3D('',#16447,#13532,#13533);
#10865=AXIS2_PLACEMENT_3D('',#16448,#13534,#13535);
#10866=AXIS2_PLACEMENT_3D('',#16449,#13536,#13537);
#10867=AXIS2_PLACEMENT_3D('',#16450,#13538,#13539);
#10868=AXIS2_PLACEMENT_3D('',#16451,#13540,#13541);
#10869=AXIS2_PLACEMENT_3D('',#16453,#13542,#13543);
#10870=AXIS2_PLACEMENT_3D('',#16456,#13545,#13546);
#10871=AXIS2_PLACEMENT_3D('',#16457,#13547,#13548);
#10872=AXIS2_PLACEMENT_3D('',#16459,#13549,#13550);
#10873=AXIS2_PLACEMENT_3D('',#16462,#13552,#13553);
#10874=AXIS2_PLACEMENT_3D('',#16463,#13554,#13555);
#10875=AXIS2_PLACEMENT_3D('',#16476,#13562,#13563);
#10876=AXIS2_PLACEMENT_3D('',#16477,#13564,#13565);
#10877=AXIS2_PLACEMENT_3D('',#16478,#13566,#13567);
#10878=AXIS2_PLACEMENT_3D('',#16484,#13571,#13572);
#10879=AXIS2_PLACEMENT_3D('',#16488,#13575,#13576);
#10880=AXIS2_PLACEMENT_3D('',#16492,#13579,#13580);
#10881=AXIS2_PLACEMENT_3D('',#16496,#13583,#13584);
#10882=AXIS2_PLACEMENT_3D('',#16500,#13587,#13588);
#10883=AXIS2_PLACEMENT_3D('',#16502,#13590,#13591);
#10884=AXIS2_PLACEMENT_3D('',#16503,#13592,#13593);
#10885=AXIS2_PLACEMENT_3D('',#16504,#13594,#13595);
#10886=AXIS2_PLACEMENT_3D('',#16505,#13596,#13597);
#10887=AXIS2_PLACEMENT_3D('',#16506,#13598,#13599);
#10888=AXIS2_PLACEMENT_3D('',#16507,#13600,#13601);
#10889=AXIS2_PLACEMENT_3D('',#16508,#13602,#13603);
#10890=AXIS2_PLACEMENT_3D('',#16509,#13604,#13605);
#10891=AXIS2_PLACEMENT_3D('',#16510,#13606,#13607);
#10892=AXIS2_PLACEMENT_3D('',#16511,#13608,#13609);
#10893=AXIS2_PLACEMENT_3D('',#16512,#13610,#13611);
#10894=AXIS2_PLACEMENT_3D('',#16513,#13612,#13613);
#10895=AXIS2_PLACEMENT_3D('',#16514,#13614,#13615);
#10896=AXIS2_PLACEMENT_3D('',#16515,#13616,#13617);
#10897=AXIS2_PLACEMENT_3D('',#16516,#13618,#13619);
#10898=AXIS2_PLACEMENT_3D('',#16517,#13620,#13621);
#10899=AXIS2_PLACEMENT_3D('',#16518,#13622,#13623);
#10900=AXIS2_PLACEMENT_3D('',#16519,#13624,#13625);
#10901=AXIS2_PLACEMENT_3D('',#16520,#13626,#13627);
#10902=AXIS2_PLACEMENT_3D('',#16521,#13628,#13629);
#10903=AXIS2_PLACEMENT_3D('',#16522,#13630,#13631);
#10904=AXIS2_PLACEMENT_3D('',#16523,#13632,#13633);
#10905=AXIS2_PLACEMENT_3D('',#16524,#13634,#13635);
#10906=AXIS2_PLACEMENT_3D('',#16525,#13636,#13637);
#10907=AXIS2_PLACEMENT_3D('',#16526,#13638,#13639);
#10908=AXIS2_PLACEMENT_3D('',#16527,#13640,#13641);
#10909=AXIS2_PLACEMENT_3D('',#16528,#13642,#13643);
#10910=AXIS2_PLACEMENT_3D('',#16529,#13644,#13645);
#10911=AXIS2_PLACEMENT_3D('',#16530,#13646,#13647);
#10912=AXIS2_PLACEMENT_3D('',#16531,#13648,#13649);
#10913=AXIS2_PLACEMENT_3D('',#16532,#13650,#13651);
#10914=AXIS2_PLACEMENT_3D('',#16533,#13652,#13653);
#10915=AXIS2_PLACEMENT_3D('',#16534,#13654,#13655);
#10916=AXIS2_PLACEMENT_3D('',#16535,#13656,#13657);
#10917=AXIS2_PLACEMENT_3D('',#16536,#13658,#13659);
#10918=AXIS2_PLACEMENT_3D('',#16537,#13660,#13661);
#10919=AXIS2_PLACEMENT_3D('',#16538,#13662,#13663);
#10920=AXIS2_PLACEMENT_3D('',#16539,#13664,#13665);
#10921=AXIS2_PLACEMENT_3D('',#16540,#13666,#13667);
#10922=AXIS2_PLACEMENT_3D('',#16541,#13668,#13669);
#10923=AXIS2_PLACEMENT_3D('',#16542,#13670,#13671);
#10924=AXIS2_PLACEMENT_3D('',#16543,#13672,#13673);
#10925=AXIS2_PLACEMENT_3D('',#16544,#13674,#13675);
#10926=AXIS2_PLACEMENT_3D('',#16545,#13676,#13677);
#10927=AXIS2_PLACEMENT_3D('',#16546,#13678,#13679);
#10928=DIRECTION('axis',(0.,0.,1.));
#10929=DIRECTION('refdir',(1.,0.,0.));
#10930=DIRECTION('axis',(0.,0.,1.));
#10931=DIRECTION('refdir',(1.,0.,0.));
#10932=DIRECTION('center_axis',(-1.,0.,0.));
#10933=DIRECTION('ref_axis',(0.,0.,1.));
#10934=DIRECTION('center_axis',(1.,0.,0.));
#10935=DIRECTION('ref_axis',(0.,0.,-1.));
#10936=DIRECTION('',(-1.,0.,0.));
#10937=DIRECTION('center_axis',(-1.,0.,0.));
#10938=DIRECTION('ref_axis',(0.,0.,-1.));
#10939=DIRECTION('center_axis',(-1.,0.,0.));
#10940=DIRECTION('ref_axis',(0.,0.,1.));
#10941=DIRECTION('center_axis',(1.,0.,0.));
#10942=DIRECTION('ref_axis',(0.,0.,-1.));
#10943=DIRECTION('',(-1.,0.,0.));
#10944=DIRECTION('center_axis',(1.,0.,0.));
#10945=DIRECTION('ref_axis',(0.,0.,1.));
#10946=DIRECTION('center_axis',(0.,0.,-1.));
#10947=DIRECTION('ref_axis',(-1.,0.,0.));
#10948=DIRECTION('',(1.,0.,0.));
#10949=DIRECTION('',(0.,-1.,0.));
#10950=DIRECTION('',(1.,0.,0.));
#10951=DIRECTION('',(0.,-1.,0.));
#10952=DIRECTION('',(-1.,0.,0.));
#10953=DIRECTION('',(0.,1.,0.));
#10954=DIRECTION('',(1.,0.,0.));
#10955=DIRECTION('',(0.,-1.,0.));
#10956=DIRECTION('',(-1.,0.,0.));
#10957=DIRECTION('',(0.,1.,0.));
#10958=DIRECTION('',(1.,0.,0.));
#10959=DIRECTION('',(0.,-1.,0.));
#10960=DIRECTION('',(-1.,0.,0.));
#10961=DIRECTION('',(0.,1.,0.));
#10962=DIRECTION('',(1.,0.,0.));
#10963=DIRECTION('',(0.,1.,0.));
#10964=DIRECTION('',(-1.,0.,0.));
#10965=DIRECTION('',(0.,1.,0.));
#10966=DIRECTION('',(1.,0.,0.));
#10967=DIRECTION('',(0.,-1.,0.));
#10968=DIRECTION('',(-1.,0.,0.));
#10969=DIRECTION('',(0.,1.,0.));
#10970=DIRECTION('',(1.,0.,0.));
#10971=DIRECTION('',(0.,-1.,0.));
#10972=DIRECTION('',(-1.,0.,0.));
#10973=DIRECTION('',(0.,1.,0.));
#10974=DIRECTION('',(1.,0.,0.));
#10975=DIRECTION('',(0.,-1.,0.));
#10976=DIRECTION('',(-1.,0.,0.));
#10977=DIRECTION('',(0.,-1.,0.));
#10978=DIRECTION('',(-1.,0.,0.));
#10979=DIRECTION('',(0.,-1.,0.));
#10980=DIRECTION('',(0.,1.,0.));
#10981=DIRECTION('',(-1.,0.,0.));
#10982=DIRECTION('',(0.,1.,0.));
#10983=DIRECTION('',(-1.,0.,0.));
#10984=DIRECTION('',(-1.,0.,0.));
#10985=DIRECTION('',(0.,1.,0.));
#10986=DIRECTION('',(-1.,0.,0.));
#10987=DIRECTION('',(0.,1.,0.));
#10988=DIRECTION('center_axis',(0.,-1.,0.));
#10989=DIRECTION('ref_axis',(0.,0.,-1.));
#10990=DIRECTION('',(0.,0.,-1.));
#10991=DIRECTION('',(0.,0.,1.));
#10992=DIRECTION('',(-1.,0.,0.));
#10993=DIRECTION('center_axis',(0.,-1.,0.));
#10994=DIRECTION('ref_axis',(0.,0.,-1.));
#10995=DIRECTION('',(0.,0.,1.));
#10996=DIRECTION('',(-1.,0.,0.));
#10997=DIRECTION('',(0.,0.,-1.));
#10998=DIRECTION('center_axis',(0.,-1.,0.));
#10999=DIRECTION('ref_axis',(0.,0.,-1.));
#11000=DIRECTION('',(0.,0.,1.));
#11001=DIRECTION('',(-1.,0.,0.));
#11002=DIRECTION('',(0.,0.,-1.));
#11003=DIRECTION('center_axis',(0.,-1.,0.));
#11004=DIRECTION('ref_axis',(0.,0.,-1.));
#11005=DIRECTION('',(0.,0.,-1.));
#11006=DIRECTION('',(0.,0.,-1.));
#11007=DIRECTION('',(-1.,0.,0.));
#11008=DIRECTION('center_axis',(0.,1.,0.));
#11009=DIRECTION('ref_axis',(0.,0.,1.));
#11010=DIRECTION('',(0.,0.,1.));
#11011=DIRECTION('',(1.,0.,0.));
#11012=DIRECTION('',(0.,0.,-1.));
#11013=DIRECTION('center_axis',(0.,1.,0.));
#11014=DIRECTION('ref_axis',(0.,0.,1.));
#11015=DIRECTION('',(0.,0.,-1.));
#11016=DIRECTION('',(0.,0.,1.));
#11017=DIRECTION('',(1.,0.,0.));
#11018=DIRECTION('center_axis',(0.,1.,0.));
#11019=DIRECTION('ref_axis',(0.,0.,1.));
#11020=DIRECTION('',(0.,0.,-1.));
#11021=DIRECTION('',(0.,0.,1.));
#11022=DIRECTION('',(1.,0.,0.));
#11023=DIRECTION('center_axis',(0.,1.,0.));
#11024=DIRECTION('ref_axis',(0.,0.,1.));
#11025=DIRECTION('',(0.,0.,-1.));
#11026=DIRECTION('',(0.,0.,-1.));
#11027=DIRECTION('',(1.,0.,0.));
#11028=DIRECTION('center_axis',(0.,0.,-1.));
#11029=DIRECTION('ref_axis',(-1.,0.,0.));
#11030=DIRECTION('',(0.,1.,0.));
#11031=DIRECTION('',(-1.,0.,0.));
#11032=DIRECTION('',(0.,-1.,0.));
#11033=DIRECTION('',(0.,1.,0.));
#11034=DIRECTION('',(-1.,0.,0.));
#11035=DIRECTION('',(0.,-1.,0.));
#11036=DIRECTION('',(0.,1.,0.));
#11037=DIRECTION('',(-1.,0.,0.));
#11038=DIRECTION('',(0.,-1.,0.));
#11039=DIRECTION('',(0.,-1.,0.));
#11040=DIRECTION('',(0.,-1.,0.));
#11041=DIRECTION('',(1.,0.,0.));
#11042=DIRECTION('',(0.,1.,0.));
#11043=DIRECTION('',(0.,-1.,0.));
#11044=DIRECTION('',(1.,0.,0.));
#11045=DIRECTION('',(0.,1.,0.));
#11046=DIRECTION('',(0.,-1.,0.));
#11047=DIRECTION('',(1.,0.,0.));
#11048=DIRECTION('',(0.,1.,0.));
#11049=DIRECTION('',(0.,1.,0.));
#11050=DIRECTION('center_axis',(-1.,0.,0.));
#11051=DIRECTION('ref_axis',(0.,0.,1.));
#11052=DIRECTION('center_axis',(1.,0.,0.));
#11053=DIRECTION('ref_axis',(0.,0.,-1.));
#11054=DIRECTION('center_axis',(-1.,0.,0.));
#11055=DIRECTION('ref_axis',(0.,0.,-1.));
#11056=DIRECTION('center_axis',(0.,1.,0.));
#11057=DIRECTION('ref_axis',(0.,0.,1.));
#11058=DIRECTION('',(0.,0.,-1.));
#11059=DIRECTION('',(0.,0.,-1.));
#11060=DIRECTION('',(-1.,0.,0.));
#11061=DIRECTION('center_axis',(0.,-1.,0.));
#11062=DIRECTION('ref_axis',(0.,0.,-1.));
#11063=DIRECTION('',(0.,0.,1.));
#11064=DIRECTION('',(-1.,0.,0.));
#11065=DIRECTION('',(0.,0.,1.));
#11066=DIRECTION('center_axis',(0.,0.,-1.));
#11067=DIRECTION('ref_axis',(-1.,0.,0.));
#11068=DIRECTION('',(0.,-1.,0.));
#11069=DIRECTION('',(-1.,0.,0.));
#11070=DIRECTION('',(0.,-1.,0.));
#11071=DIRECTION('center_axis',(0.,0.832050294337844,0.554700196225229));
#11072=DIRECTION('ref_axis',(0.,-0.554700196225229,0.832050294337844));
#11073=DIRECTION('',(0.,0.554700196225229,-0.832050294337844));
#11074=DIRECTION('',(0.,0.554700196225229,-0.832050294337844));
#11075=DIRECTION('center_axis',(1.,0.,0.));
#11076=DIRECTION('ref_axis',(0.,0.,-1.));
#11077=DIRECTION('center_axis',(1.,0.,0.));
#11078=DIRECTION('ref_axis',(0.,0.,-1.));
#11079=DIRECTION('center_axis',(0.,-1.,0.));
#11080=DIRECTION('ref_axis',(0.,0.,-1.));
#11081=DIRECTION('',(0.,0.,1.));
#11082=DIRECTION('',(-1.,0.,0.));
#11083=DIRECTION('',(0.,0.,1.));
#11084=DIRECTION('center_axis',(0.,-0.832050294337844,0.554700196225229));
#11085=DIRECTION('ref_axis',(0.,-0.554700196225229,-0.832050294337844));
#11086=DIRECTION('',(0.,0.554700196225229,0.832050294337844));
#11087=DIRECTION('',(-1.,0.,0.));
#11088=DIRECTION('',(0.,0.554700196225229,0.832050294337844));
#11089=DIRECTION('center_axis',(0.,0.,-1.));
#11090=DIRECTION('ref_axis',(-1.,0.,0.));
#11091=DIRECTION('',(0.,-1.,0.));
#11092=DIRECTION('',(-1.,0.,0.));
#11093=DIRECTION('',(0.,-1.,0.));
#11094=DIRECTION('center_axis',(0.,1.,0.));
#11095=DIRECTION('ref_axis',(0.,0.,1.));
#11096=DIRECTION('',(0.,0.,-1.));
#11097=DIRECTION('',(0.,0.,-1.));
#11098=DIRECTION('center_axis',(-1.,0.,0.));
#11099=DIRECTION('ref_axis',(0.,0.,1.));
#11100=DIRECTION('center_axis',(-1.,0.,0.));
#11101=DIRECTION('ref_axis',(0.,0.,1.));
#11102=DIRECTION('center_axis',(-1.,0.,0.));
#11103=DIRECTION('ref_axis',(0.,0.,1.));
#11104=DIRECTION('',(0.,0.,-1.));
#11105=DIRECTION('center_axis',(0.,-1.,0.));
#11106=DIRECTION('ref_axis',(0.,0.,-1.));
#11107=DIRECTION('',(0.,0.,-1.));
#11108=DIRECTION('center_axis',(1.,0.,0.));
#11109=DIRECTION('ref_axis',(0.,0.,-1.));
#11110=DIRECTION('center_axis',(-1.,0.,0.));
#11111=DIRECTION('ref_axis',(0.,0.,1.));
#11112=DIRECTION('',(0.,0.,-1.));
#11113=DIRECTION('center_axis',(1.,0.,0.));
#11114=DIRECTION('ref_axis',(0.,0.,-1.));
#11115=DIRECTION('',(0.,0.,-1.));
#11116=DIRECTION('center_axis',(0.,1.,0.));
#11117=DIRECTION('ref_axis',(0.,0.,1.));
#11118=DIRECTION('center_axis',(-1.,0.,0.));
#11119=DIRECTION('ref_axis',(0.,0.,1.));
#11120=DIRECTION('',(0.,0.,-1.));
#11121=DIRECTION('center_axis',(1.,0.,0.));
#11122=DIRECTION('ref_axis',(0.,0.,-1.));
#11123=DIRECTION('',(0.,0.,-1.));
#11124=DIRECTION('center_axis',(0.,1.,0.));
#11125=DIRECTION('ref_axis',(0.,0.,1.));
#11126=DIRECTION('center_axis',(-1.,0.,0.));
#11127=DIRECTION('ref_axis',(0.,0.,1.));
#11128=DIRECTION('',(0.,0.,-1.));
#11129=DIRECTION('center_axis',(0.,-1.,0.));
#11130=DIRECTION('ref_axis',(0.,0.,-1.));
#11131=DIRECTION('',(0.,0.,-1.));
#11132=DIRECTION('center_axis',(1.,0.,0.));
#11133=DIRECTION('ref_axis',(0.,0.,-1.));
#11134=DIRECTION('center_axis',(-1.,0.,0.));
#11135=DIRECTION('ref_axis',(0.,0.,1.));
#11136=DIRECTION('',(0.,0.,-1.));
#11137=DIRECTION('center_axis',(1.,0.,0.));
#11138=DIRECTION('ref_axis',(0.,0.,-1.));
#11139=DIRECTION('',(0.,0.,-1.));
#11140=DIRECTION('center_axis',(0.,1.,0.));
#11141=DIRECTION('ref_axis',(0.,0.,1.));
#11142=DIRECTION('center_axis',(-1.,0.,0.));
#11143=DIRECTION('ref_axis',(0.,0.,1.));
#11144=DIRECTION('',(0.,0.,-1.));
#11145=DIRECTION('center_axis',(0.,-1.,0.));
#11146=DIRECTION('ref_axis',(0.,0.,-1.));
#11147=DIRECTION('',(0.,0.,-1.));
#11148=DIRECTION('center_axis',(1.,0.,0.));
#11149=DIRECTION('ref_axis',(0.,0.,-1.));
#11150=DIRECTION('center_axis',(1.,0.,0.));
#11151=DIRECTION('ref_axis',(0.,0.,-1.));
#11152=DIRECTION('center_axis',(1.,0.,0.));
#11153=DIRECTION('ref_axis',(0.,0.,-1.));
#11154=DIRECTION('center_axis',(1.,0.,0.));
#11155=DIRECTION('ref_axis',(0.,0.,-1.));
#11156=DIRECTION('center_axis',(1.,0.,0.));
#11157=DIRECTION('ref_axis',(0.,0.,-1.));
#11158=DIRECTION('center_axis',(-1.,0.,0.));
#11159=DIRECTION('ref_axis',(0.,-1.22464679914735E-16,-1.));
#11160=DIRECTION('axis',(0.,0.,1.));
#11161=DIRECTION('refdir',(1.,0.,0.));
#11162=DIRECTION('center_axis',(0.,-1.,0.));
#11163=DIRECTION('ref_axis',(0.,0.,-1.));
#11164=DIRECTION('center_axis',(0.,1.,0.));
#11165=DIRECTION('ref_axis',(2.66453525910038E-15,0.,-1.));
#11166=DIRECTION('',(0.,-1.,0.));
#11167=DIRECTION('center_axis',(0.,1.,0.));
#11168=DIRECTION('ref_axis',(0.,0.,1.));
#11169=DIRECTION('',(0.,1.,0.));
#11170=DIRECTION('center_axis',(0.,-1.,0.));
#11171=DIRECTION('ref_axis',(0.,0.,-1.));
#11172=DIRECTION('center_axis',(0.,1.,0.));
#11173=DIRECTION('ref_axis',(0.,0.,-1.));
#11174=DIRECTION('',(0.,-1.,0.));
#11175=DIRECTION('center_axis',(0.,1.,0.));
#11176=DIRECTION('ref_axis',(0.,0.,1.));
#11177=DIRECTION('center_axis',(0.,-1.,0.));
#11178=DIRECTION('ref_axis',(0.,0.,-1.));
#11179=DIRECTION('center_axis',(0.,-1.,0.));
#11180=DIRECTION('ref_axis',(0.,0.,1.));
#11181=DIRECTION('',(0.,-1.,0.));
#11182=DIRECTION('center_axis',(0.,1.,0.));
#11183=DIRECTION('ref_axis',(0.,0.,1.));
#11184=DIRECTION('center_axis',(0.,-1.,0.));
#11185=DIRECTION('ref_axis',(0.,0.,-1.));
#11186=DIRECTION('center_axis',(0.,1.,0.));
#11187=DIRECTION('ref_axis',(0.,0.,-1.));
#11188=DIRECTION('',(0.,-1.,0.));
#11189=DIRECTION('center_axis',(3.03770030380451E-15,-0.832050294337844,
0.554700196225228));
#11190=DIRECTION('ref_axis',(-6.45395818566141E-13,-0.554700196225228,-0.832050294337844));
#11191=DIRECTION('center_axis',(0.,1.,0.));
#11192=DIRECTION('ref_axis',(0.,0.,1.));
#11193=DIRECTION('center_axis',(3.03770030380451E-15,-0.832050294337844,
0.554700196225228));
#11194=DIRECTION('ref_axis',(-6.45395818566141E-13,-0.554700196225228,-0.832050294337844));
#11195=DIRECTION('center_axis',(0.,-1.,0.));
#11196=DIRECTION('ref_axis',(0.,0.,-1.));
#11197=DIRECTION('center_axis',(0.,1.,0.));
#11198=DIRECTION('ref_axis',(0.,0.,-1.));
#11199=DIRECTION('',(0.,-1.,0.));
#11200=DIRECTION('center_axis',(-2.10302328724925E-15,-0.832050294337843,
0.554700196225231));
#11201=DIRECTION('ref_axis',(-1.7015761927577E-13,-0.55470019622523,-0.832050294337843));
#11202=DIRECTION('center_axis',(0.,1.,0.));
#11203=DIRECTION('ref_axis',(0.,0.,1.));
#11204=DIRECTION('center_axis',(-2.10302328724925E-15,-0.832050294337843,
0.554700196225231));
#11205=DIRECTION('ref_axis',(-1.7015761927577E-13,-0.55470019622523,-0.832050294337843));
#11206=DIRECTION('center_axis',(0.,-1.,0.));
#11207=DIRECTION('ref_axis',(0.,0.,-1.));
#11208=DIRECTION('center_axis',(0.,1.,0.));
#11209=DIRECTION('ref_axis',(0.,0.,-1.));
#11210=DIRECTION('',(0.,-1.,0.));
#11211=DIRECTION('center_axis',(3.0377003038045E-15,-0.832050294337844,
0.554700196225229));
#11212=DIRECTION('ref_axis',(4.33987867344828E-14,-0.554700196225228,-0.832050294337844));
#11213=DIRECTION('center_axis',(0.,1.,0.));
#11214=DIRECTION('ref_axis',(0.,0.,1.));
#11215=DIRECTION('center_axis',(3.0377003038045E-15,-0.832050294337844,
0.554700196225229));
#11216=DIRECTION('ref_axis',(4.33987867344828E-14,-0.554700196225228,-0.832050294337844));
#11217=DIRECTION('center_axis',(0.,0.,-1.));
#11218=DIRECTION('ref_axis',(-1.,0.,0.));
#11219=DIRECTION('',(1.,0.,0.));
#11220=DIRECTION('',(-1.,0.,0.));
#11221=DIRECTION('',(0.,-1.,0.));
#11222=DIRECTION('',(-1.,0.,0.));
#11223=DIRECTION('',(0.,-1.,0.));
#11224=DIRECTION('',(-1.,0.,0.));
#11225=DIRECTION('',(-1.,0.,0.));
#11226=DIRECTION('',(0.,-1.,0.));
#11227=DIRECTION('',(-1.,0.,0.));
#11228=DIRECTION('',(0.,-1.,0.));
#11229=DIRECTION('',(0.,-1.,0.));
#11230=DIRECTION('',(-1.,0.,0.));
#11231=DIRECTION('',(0.,-1.,0.));
#11232=DIRECTION('',(-1.,0.,0.));
#11233=DIRECTION('center_axis',(0.,0.832050294337844,-0.554700196225229));
#11234=DIRECTION('ref_axis',(0.,0.554700196225229,0.832050294337844));
#11235=DIRECTION('',(0.,-0.554700196225229,-0.832050294337844));
#11236=DIRECTION('',(-1.,0.,0.));
#11237=DIRECTION('',(0.,-0.554700196225229,-0.832050294337844));
#11238=DIRECTION('',(-1.,0.,0.));
#11239=DIRECTION('',(1.,0.,0.));
#11240=DIRECTION('',(1.,0.,0.));
#11241=DIRECTION('',(1.,0.,0.));
#11242=DIRECTION('center_axis',(0.,1.,0.));
#11243=DIRECTION('ref_axis',(0.,0.,1.));
#11244=DIRECTION('',(0.,0.,-1.));
#11245=DIRECTION('',(-1.,0.,0.));
#11246=DIRECTION('',(0.,0.,-1.));
#11247=DIRECTION('center_axis',(0.,0.,1.));
#11248=DIRECTION('ref_axis',(1.,0.,0.));
#11249=DIRECTION('',(0.,1.,0.));
#11250=DIRECTION('',(-1.,0.,0.));
#11251=DIRECTION('',(0.,1.,0.));
#11252=DIRECTION('center_axis',(0.,1.,0.));
#11253=DIRECTION('ref_axis',(0.,0.,1.));
#11254=DIRECTION('',(0.,0.,-1.));
#11255=DIRECTION('',(-1.,0.,0.));
#11256=DIRECTION('',(0.,0.,-1.));
#11257=DIRECTION('center_axis',(0.,0.,1.));
#11258=DIRECTION('ref_axis',(1.,0.,0.));
#11259=DIRECTION('',(0.,1.,0.));
#11260=DIRECTION('',(-1.,0.,0.));
#11261=DIRECTION('',(0.,1.,0.));
#11262=DIRECTION('center_axis',(0.,-0.832050294337844,-0.554700196225229));
#11263=DIRECTION('ref_axis',(0.,0.554700196225229,-0.832050294337843));
#11264=DIRECTION('',(0.,-0.554700196225229,0.832050294337843));
#11265=DIRECTION('',(-1.,0.,0.));
#11266=DIRECTION('',(0.,-0.554700196225229,0.832050294337843));
#11267=DIRECTION('center_axis',(0.,0.,1.));
#11268=DIRECTION('ref_axis',(1.,0.,0.));
#11269=DIRECTION('',(0.,1.,0.));
#11270=DIRECTION('',(0.,1.,0.));
#11271=DIRECTION('center_axis',(0.,0.,1.));
#11272=DIRECTION('ref_axis',(1.,0.,0.));
#11273=DIRECTION('',(0.,1.,0.));
#11274=DIRECTION('',(-1.,0.,0.));
#11275=DIRECTION('',(0.,1.,0.));
#11276=DIRECTION('center_axis',(0.,-1.,0.));
#11277=DIRECTION('ref_axis',(0.,0.,-1.));
#11278=DIRECTION('',(0.,0.,1.));
#11279=DIRECTION('',(-1.,0.,0.));
#11280=DIRECTION('',(0.,0.,1.));
#11281=DIRECTION('center_axis',(0.,0.,1.));
#11282=DIRECTION('ref_axis',(1.,0.,0.));
#11283=DIRECTION('',(0.,1.,0.));
#11284=DIRECTION('',(-1.,0.,0.));
#11285=DIRECTION('',(0.,1.,0.));
#11286=DIRECTION('center_axis',(0.,-1.,0.));
#11287=DIRECTION('ref_axis',(0.,0.,-1.));
#11288=DIRECTION('',(0.,0.,1.));
#11289=DIRECTION('',(0.,0.,1.));
#11290=DIRECTION('center_axis',(1.,0.,0.));
#11291=DIRECTION('ref_axis',(0.,0.,-1.));
#11292=DIRECTION('center_axis',(1.,0.,0.));
#11293=DIRECTION('ref_axis',(0.,0.,-1.));
#11294=DIRECTION('center_axis',(1.,0.,0.));
#11295=DIRECTION('ref_axis',(0.,0.,-1.));
#11296=DIRECTION('',(0.,0.,1.));
#11297=DIRECTION('',(0.,-1.,0.));
#11298=DIRECTION('',(0.,0.,1.));
#11299=DIRECTION('center_axis',(0.832050294337844,0.,0.554700196225229));
#11300=DIRECTION('ref_axis',(0.554700196225229,0.,-0.832050294337844));
#11301=DIRECTION('',(-0.554700196225229,0.,0.832050294337844));
#11302=DIRECTION('',(0.,-1.,0.));
#11303=DIRECTION('',(-0.554700196225229,0.,0.832050294337844));
#11304=DIRECTION('center_axis',(0.,0.,-1.));
#11305=DIRECTION('ref_axis',(-1.,0.,0.));
#11306=DIRECTION('',(1.,0.,0.));
#11307=DIRECTION('',(0.,-1.,0.));
#11308=DIRECTION('',(1.,0.,0.));
#11309=DIRECTION('center_axis',(-1.,0.,0.));
#11310=DIRECTION('ref_axis',(0.,0.,1.));
#11311=DIRECTION('',(0.,0.,-1.));
#11312=DIRECTION('',(0.,0.,-1.));
#11313=DIRECTION('center_axis',(0.,-1.,0.));
#11314=DIRECTION('ref_axis',(0.,0.,-1.));
#11315=DIRECTION('center_axis',(0.,-1.,0.));
#11316=DIRECTION('ref_axis',(0.,0.,-1.));
#11317=DIRECTION('center_axis',(-1.,0.,0.));
#11318=DIRECTION('ref_axis',(0.,0.,1.));
#11319=DIRECTION('',(0.,0.,-1.));
#11320=DIRECTION('',(0.,0.,-1.));
#11321=DIRECTION('',(0.,-1.,0.));
#11322=DIRECTION('center_axis',(1.,0.,0.));
#11323=DIRECTION('ref_axis',(0.,0.,-1.));
#11324=DIRECTION('',(0.,0.,1.));
#11325=DIRECTION('',(0.,-1.,0.));
#11326=DIRECTION('',(0.,0.,1.));
#11327=DIRECTION('center_axis',(0.,0.,-1.));
#11328=DIRECTION('ref_axis',(-1.,0.,0.));
#11329=DIRECTION('',(1.,0.,0.));
#11330=DIRECTION('',(0.,-1.,0.));
#11331=DIRECTION('',(1.,0.,0.));
#11332=DIRECTION('center_axis',(-0.832050294337844,0.,0.554700196225229));
#11333=DIRECTION('ref_axis',(0.554700196225229,0.,0.832050294337844));
#11334=DIRECTION('',(-0.554700196225229,0.,-0.832050294337844));
#11335=DIRECTION('',(-0.554700196225229,0.,-0.832050294337844));
#11336=DIRECTION('center_axis',(0.,1.,0.));
#11337=DIRECTION('ref_axis',(0.,0.,1.));
#11338=DIRECTION('center_axis',(0.,1.,0.));
#11339=DIRECTION('ref_axis',(0.,0.,1.));
#11340=DIRECTION('center_axis',(0.,1.,0.));
#11341=DIRECTION('ref_axis',(0.,0.,1.));
#11342=DIRECTION('center_axis',(0.,1.,0.));
#11343=DIRECTION('ref_axis',(0.,0.,1.));
#11344=DIRECTION('center_axis',(0.,1.,0.));
#11345=DIRECTION('ref_axis',(0.,0.,1.));
#11346=DIRECTION('center_axis',(0.,1.,0.));
#11347=DIRECTION('ref_axis',(0.,0.,1.));
#11348=DIRECTION('center_axis',(0.,1.,0.));
#11349=DIRECTION('ref_axis',(0.,0.,1.));
#11350=DIRECTION('center_axis',(0.,1.,0.));
#11351=DIRECTION('ref_axis',(0.,0.,1.));
#11352=DIRECTION('axis',(0.,0.,1.));
#11353=DIRECTION('refdir',(1.,0.,0.));
#11354=DIRECTION('center_axis',(-1.,0.,0.));
#11355=DIRECTION('ref_axis',(0.,0.,1.));
#11356=DIRECTION('center_axis',(1.,0.,0.));
#11357=DIRECTION('ref_axis',(0.,0.,1.));
#11358=DIRECTION('',(-1.,0.,0.));
#11359=DIRECTION('center_axis',(1.,0.,0.));
#11360=DIRECTION('ref_axis',(0.,0.,-1.));
#11361=DIRECTION('center_axis',(-0.832050294337839,-8.41209314899718E-15,
0.554700196225236));
#11362=DIRECTION('ref_axis',(0.554700196225236,1.57539479552213E-13,0.832050294337839));
#11363=DIRECTION('center_axis',(1.,0.,0.));
#11364=DIRECTION('ref_axis',(0.,0.,-1.));
#11365=DIRECTION('center_axis',(-1.,0.,0.));
#11366=DIRECTION('ref_axis',(0.,0.,1.));
#11367=DIRECTION('center_axis',(1.,0.,0.));
#11368=DIRECTION('ref_axis',(0.,0.,1.));
#11369=DIRECTION('',(-1.,0.,0.));
#11370=DIRECTION('center_axis',(1.,0.,0.));
#11371=DIRECTION('ref_axis',(0.,0.,-1.));
#11372=DIRECTION('center_axis',(-0.832050294337839,-8.56787265175636E-15,
0.554700196225237));
#11373=DIRECTION('ref_axis',(0.554700196225236,7.46312953944725E-13,0.832050294337839));
#11374=DIRECTION('center_axis',(1.,0.,0.));
#11375=DIRECTION('ref_axis',(0.,0.,-1.));
#11376=DIRECTION('center_axis',(-1.,0.,0.));
#11377=DIRECTION('ref_axis',(0.,0.,1.));
#11378=DIRECTION('center_axis',(1.,0.,0.));
#11379=DIRECTION('ref_axis',(0.,0.,1.));
#11380=DIRECTION('',(-1.,0.,0.));
#11381=DIRECTION('center_axis',(1.,0.,0.));
#11382=DIRECTION('ref_axis',(0.,0.,-1.));
#11383=DIRECTION('center_axis',(-0.832050294337839,-8.56787265175632E-15,
0.554700196225236));
#11384=DIRECTION('ref_axis',(0.554700196225236,4.28606070402036E-13,0.832050294337839));
#11385=DIRECTION('center_axis',(1.,0.,0.));
#11386=DIRECTION('ref_axis',(0.,0.,-1.));
#11387=DIRECTION('center_axis',(0.,-1.,0.));
#11388=DIRECTION('ref_axis',(0.,0.,-1.));
#11389=DIRECTION('center_axis',(0.,1.,0.));
#11390=DIRECTION('ref_axis',(0.,0.,1.));
#11391=DIRECTION('',(0.,-1.,0.));
#11392=DIRECTION('center_axis',(0.,1.,0.));
#11393=DIRECTION('ref_axis',(0.,0.,-1.));
#11394=DIRECTION('center_axis',(0.,-1.,0.));
#11395=DIRECTION('ref_axis',(0.,0.,-1.));
#11396=DIRECTION('center_axis',(0.,1.,0.));
#11397=DIRECTION('ref_axis',(0.,0.,1.));
#11398=DIRECTION('',(0.,-1.,0.));
#11399=DIRECTION('center_axis',(0.,1.,0.));
#11400=DIRECTION('ref_axis',(0.,0.,-1.));
#11401=DIRECTION('center_axis',(0.,-1.,0.));
#11402=DIRECTION('ref_axis',(0.,0.,-1.));
#11403=DIRECTION('center_axis',(0.,1.,0.));
#11404=DIRECTION('ref_axis',(0.,0.,-1.));
#11405=DIRECTION('',(0.,-1.,0.));
#11406=DIRECTION('center_axis',(0.,-1.,0.));
#11407=DIRECTION('ref_axis',(0.,0.,1.));
#11408=DIRECTION('center_axis',(0.,0.,-1.));
#11409=DIRECTION('ref_axis',(-1.,0.,0.));
#11410=DIRECTION('',(0.,-1.,0.));
#11411=DIRECTION('',(-1.,0.,0.));
#11412=DIRECTION('',(0.,-1.,0.));
#11413=DIRECTION('',(1.,0.,0.));
#11414=DIRECTION('',(0.,-1.,0.));
#11415=DIRECTION('',(-1.,0.,0.));
#11416=DIRECTION('',(0.,-1.,0.));
#11417=DIRECTION('',(-1.,0.,0.));
#11418=DIRECTION('',(0.,-1.,0.));
#11419=DIRECTION('',(-1.,0.,0.));
#11420=DIRECTION('',(0.,-1.,0.));
#11421=DIRECTION('',(1.,0.,0.));
#11422=DIRECTION('',(1.,0.,0.));
#11423=DIRECTION('',(0.,1.,0.));
#11424=DIRECTION('',(-1.,0.,0.));
#11425=DIRECTION('',(0.,-1.,0.));
#11426=DIRECTION('',(1.,0.,0.));
#11427=DIRECTION('',(0.,-1.,0.));
#11428=DIRECTION('',(-1.,0.,0.));
#11429=DIRECTION('',(0.,-1.,0.));
#11430=DIRECTION('',(-1.,0.,0.));
#11431=DIRECTION('',(0.,1.,0.));
#11432=DIRECTION('',(-1.,0.,0.));
#11433=DIRECTION('',(0.,1.,0.));
#11434=DIRECTION('center_axis',(0.,-1.,0.));
#11435=DIRECTION('ref_axis',(0.,0.,-1.));
#11436=DIRECTION('',(-1.,0.,0.));
#11437=DIRECTION('',(0.,0.,1.));
#11438=DIRECTION('',(1.,0.,0.));
#11439=DIRECTION('',(0.,0.,1.));
#11440=DIRECTION('',(-1.,0.,0.));
#11441=DIRECTION('',(0.554700196225229,0.,-0.832050294337844));
#11442=DIRECTION('',(-1.,0.,0.));
#11443=DIRECTION('',(0.554700196225229,0.,0.832050294337844));
#11444=DIRECTION('',(-1.,0.,0.));
#11445=DIRECTION('',(0.,0.,-1.));
#11446=DIRECTION('',(1.,0.,0.));
#11447=DIRECTION('',(0.,0.,-1.));
#11448=DIRECTION('center_axis',(0.,0.,-1.));
#11449=DIRECTION('ref_axis',(-1.,0.,0.));
#11450=DIRECTION('',(0.,-1.,0.));
#11451=DIRECTION('',(1.,0.,0.));
#11452=DIRECTION('',(0.,1.,0.));
#11453=DIRECTION('',(0.,1.,0.));
#11454=DIRECTION('',(1.,0.,0.));
#11455=DIRECTION('',(0.,-1.,0.));
#11456=DIRECTION('center_axis',(-1.,0.,0.));
#11457=DIRECTION('ref_axis',(0.,0.,1.));
#11458=DIRECTION('',(0.,0.,-1.));
#11459=DIRECTION('',(0.,-1.,0.));
#11460=DIRECTION('',(0.,0.,-1.));
#11461=DIRECTION('center_axis',(-1.,0.,0.));
#11462=DIRECTION('ref_axis',(0.,0.,1.));
#11463=DIRECTION('',(0.,-1.,0.));
#11464=DIRECTION('',(0.,0.,1.));
#11465=DIRECTION('',(0.,0.,-1.));
#11466=DIRECTION('center_axis',(1.,0.,0.));
#11467=DIRECTION('ref_axis',(0.,0.,-1.));
#11468=DIRECTION('',(0.,-1.,0.));
#11469=DIRECTION('',(0.,0.,1.));
#11470=DIRECTION('',(0.,0.,1.));
#11471=DIRECTION('center_axis',(1.,0.,0.));
#11472=DIRECTION('ref_axis',(0.,0.,-1.));
#11473=DIRECTION('',(0.,0.,-1.));
#11474=DIRECTION('',(0.,-1.,0.));
#11475=DIRECTION('',(0.,0.,1.));
#11476=DIRECTION('center_axis',(0.,0.,-1.));
#11477=DIRECTION('ref_axis',(-1.,0.,0.));
#11478=DIRECTION('',(1.,0.,0.));
#11479=DIRECTION('',(0.,-1.,0.));
#11480=DIRECTION('',(1.,0.,0.));
#11481=DIRECTION('center_axis',(0.,0.,-1.));
#11482=DIRECTION('ref_axis',(-1.,0.,0.));
#11483=DIRECTION('',(0.,-1.,0.));
#11484=DIRECTION('',(-1.,0.,0.));
#11485=DIRECTION('',(1.,0.,0.));
#11486=DIRECTION('center_axis',(0.,0.,1.));
#11487=DIRECTION('ref_axis',(1.,0.,0.));
#11488=DIRECTION('',(0.,-1.,0.));
#11489=DIRECTION('',(-1.,0.,0.));
#11490=DIRECTION('',(0.,-1.,0.));
#11491=DIRECTION('',(-1.,0.,0.));
#11492=DIRECTION('center_axis',(0.,0.,1.));
#11493=DIRECTION('ref_axis',(1.,0.,0.));
#11494=DIRECTION('',(0.,-1.,0.));
#11495=DIRECTION('',(1.,0.,0.));
#11496=DIRECTION('',(0.,-1.,0.));
#11497=DIRECTION('',(-1.,0.,0.));
#11498=DIRECTION('center_axis',(0.,0.,-1.));
#11499=DIRECTION('ref_axis',(-1.,0.,0.));
#11500=DIRECTION('',(0.,-1.,0.));
#11501=DIRECTION('',(1.,0.,0.));
#11502=DIRECTION('',(1.,0.,0.));
#11503=DIRECTION('center_axis',(0.,0.,-1.));
#11504=DIRECTION('ref_axis',(-1.,0.,0.));
#11505=DIRECTION('',(-1.,0.,0.));
#11506=DIRECTION('',(0.,-1.,0.));
#11507=DIRECTION('',(1.,0.,0.));
#11508=DIRECTION('center_axis',(0.832050294337844,0.,-0.554700196225229));
#11509=DIRECTION('ref_axis',(-0.554700196225229,0.,-0.832050294337844));
#11510=DIRECTION('',(0.,-1.,0.));
#11511=DIRECTION('',(0.554700196225229,0.,0.832050294337844));
#11512=DIRECTION('',(0.,-1.,0.));
#11513=DIRECTION('',(0.,-1.,0.));
#11514=DIRECTION('',(0.,-1.,0.));
#11515=DIRECTION('',(0.,-1.,0.));
#11516=DIRECTION('center_axis',(-1.,0.,0.));
#11517=DIRECTION('ref_axis',(0.,0.,1.));
#11518=DIRECTION('',(0.,0.,-1.));
#11519=DIRECTION('',(0.,1.,0.));
#11520=DIRECTION('',(0.,0.,-1.));
#11521=DIRECTION('',(0.,0.,-1.));
#11522=DIRECTION('',(0.,-1.,0.));
#11523=DIRECTION('center_axis',(0.,0.,1.));
#11524=DIRECTION('ref_axis',(1.,0.,0.));
#11525=DIRECTION('',(-1.,0.,0.));
#11526=DIRECTION('center_axis',(0.,0.,1.));
#11527=DIRECTION('ref_axis',(1.,0.,0.));
#11528=DIRECTION('',(0.,-1.,0.));
#11529=DIRECTION('',(-1.,0.,0.));
#11530=DIRECTION('center_axis',(-0.832050294337844,0.,-0.554700196225229));
#11531=DIRECTION('ref_axis',(-0.554700196225229,0.,0.832050294337844));
#11532=DIRECTION('',(0.,-1.,0.));
#11533=DIRECTION('',(0.554700196225229,0.,-0.832050294337844));
#11534=DIRECTION('center_axis',(0.,0.,1.));
#11535=DIRECTION('ref_axis',(1.,0.,0.));
#11536=DIRECTION('',(0.,-1.,0.));
#11537=DIRECTION('',(-1.,0.,0.));
#11538=DIRECTION('center_axis',(1.,0.,0.));
#11539=DIRECTION('ref_axis',(0.,0.,-1.));
#11540=DIRECTION('',(0.,0.,-1.));
#11541=DIRECTION('',(0.,0.,-1.));
#11542=DIRECTION('',(0.,-1.,0.));
#11543=DIRECTION('',(0.,0.,1.));
#11544=DIRECTION('center_axis',(0.,-1.,0.));
#11545=DIRECTION('ref_axis',(0.,0.,-1.));
#11546=DIRECTION('',(1.,0.,0.));
#11547=DIRECTION('center_axis',(0.,1.,0.));
#11548=DIRECTION('ref_axis',(0.,0.,1.));
#11549=DIRECTION('',(0.,0.,-1.));
#11550=DIRECTION('',(0.70710678118653,0.,-0.707106781186565));
#11551=DIRECTION('',(1.,0.,0.));
#11552=DIRECTION('',(0.707106781186556,0.,0.707106781186539));
#11553=DIRECTION('',(0.,0.,1.));
#11554=DIRECTION('center_axis',(0.,0.,-1.));
#11555=DIRECTION('ref_axis',(-1.,0.,0.));
#11556=DIRECTION('',(-1.,0.,0.));
#11557=DIRECTION('center_axis',(0.,-1.,0.));
#11558=DIRECTION('ref_axis',(0.,0.,-1.));
#11559=DIRECTION('',(0.,0.,1.));
#11560=DIRECTION('',(0.707106781186555,0.,0.70710678118654));
#11561=DIRECTION('',(1.,0.,0.));
#11562=DIRECTION('',(0.70710678118653,0.,-0.707106781186565));
#11563=DIRECTION('',(0.,0.,-1.));
#11564=DIRECTION('center_axis',(1.,0.,0.));
#11565=DIRECTION('ref_axis',(0.,0.,-1.));
#11566=DIRECTION('',(0.,0.,1.));
#11567=DIRECTION('',(0.,-1.,0.));
#11568=DIRECTION('center_axis',(0.70710678118654,0.,-0.707106781186555));
#11569=DIRECTION('ref_axis',(-0.707106781186555,0.,-0.70710678118654));
#11570=DIRECTION('',(0.707106781186555,0.,0.70710678118654));
#11571=DIRECTION('',(0.,-1.,0.));
#11572=DIRECTION('center_axis',(0.,0.,-1.));
#11573=DIRECTION('ref_axis',(-1.,0.,0.));
#11574=DIRECTION('',(1.,0.,0.));
#11575=DIRECTION('',(0.,-1.,0.));
#11576=DIRECTION('center_axis',(-0.707106781186565,0.,-0.70710678118653));
#11577=DIRECTION('ref_axis',(-0.70710678118653,0.,0.707106781186565));
#11578=DIRECTION('',(0.70710678118653,0.,-0.707106781186565));
#11579=DIRECTION('',(0.,-1.,0.));
#11580=DIRECTION('center_axis',(-1.,0.,0.));
#11581=DIRECTION('ref_axis',(0.,0.,1.));
#11582=DIRECTION('',(0.,0.,-1.));
#11583=DIRECTION('center_axis',(0.,-1.,0.));
#11584=DIRECTION('ref_axis',(0.,0.,-1.));
#11585=DIRECTION('center_axis',(1.,0.,0.));
#11586=DIRECTION('ref_axis',(0.,0.,-1.));
#11587=DIRECTION('',(0.,-1.,0.));
#11588=DIRECTION('',(0.,0.,1.));
#11589=DIRECTION('center_axis',(0.707106781186539,0.,-0.707106781186556));
#11590=DIRECTION('ref_axis',(-0.707106781186556,0.,-0.707106781186539));
#11591=DIRECTION('',(0.,-1.,0.));
#11592=DIRECTION('',(0.707106781186556,0.,0.707106781186539));
#11593=DIRECTION('center_axis',(0.,0.,-1.));
#11594=DIRECTION('ref_axis',(-1.,0.,0.));
#11595=DIRECTION('',(0.,-1.,0.));
#11596=DIRECTION('',(1.,0.,0.));
#11597=DIRECTION('center_axis',(-0.707106781186565,0.,-0.70710678118653));
#11598=DIRECTION('ref_axis',(-0.70710678118653,0.,0.707106781186565));
#11599=DIRECTION('',(0.,-1.,0.));
#11600=DIRECTION('',(0.70710678118653,0.,-0.707106781186565));
#11601=DIRECTION('center_axis',(-1.,0.,0.));
#11602=DIRECTION('ref_axis',(0.,0.,1.));
#11603=DIRECTION('',(0.,0.,-1.));
#11604=DIRECTION('center_axis',(0.,-1.,0.));
#11605=DIRECTION('ref_axis',(0.,0.,-1.));
#11606=DIRECTION('center_axis',(0.,-1.,0.));
#11607=DIRECTION('ref_axis',(0.,0.,-1.));
#11608=DIRECTION('',(0.,0.,1.));
#11609=DIRECTION('',(0.,0.,-1.));
#11610=DIRECTION('center_axis',(0.,-1.,0.));
#11611=DIRECTION('ref_axis',(0.,0.,-1.));
#11612=DIRECTION('',(0.,0.,-1.));
#11613=DIRECTION('',(0.,0.,1.));
#11614=DIRECTION('center_axis',(-1.,0.,0.));
#11615=DIRECTION('ref_axis',(0.,0.,1.));
#11616=DIRECTION('',(0.,0.,-1.));
#11617=DIRECTION('',(0.,0.,-1.));
#11618=DIRECTION('',(0.,0.,-1.));
#11619=DIRECTION('',(0.,0.,-1.));
#11620=DIRECTION('',(0.,1.,0.));
#11621=DIRECTION('center_axis',(1.,0.,0.));
#11622=DIRECTION('ref_axis',(0.,0.,-1.));
#11623=DIRECTION('',(0.,0.,-1.));
#11624=DIRECTION('',(0.,0.,-1.));
#11625=DIRECTION('',(0.,-1.,0.));
#11626=DIRECTION('',(0.,0.,-1.));
#11627=DIRECTION('',(0.,0.,-1.));
#11628=DIRECTION('center_axis',(0.,1.,0.));
#11629=DIRECTION('ref_axis',(0.,0.,1.));
#11630=DIRECTION('center_axis',(0.,1.,0.));
#11631=DIRECTION('ref_axis',(0.,0.,1.));
#11632=DIRECTION('center_axis',(1.,0.,0.));
#11633=DIRECTION('ref_axis',(0.,0.,-1.));
#11634=DIRECTION('center_axis',(1.,0.,0.));
#11635=DIRECTION('ref_axis',(0.,0.,-1.));
#11636=DIRECTION('center_axis',(1.,0.,0.));
#11637=DIRECTION('ref_axis',(0.,0.,-1.));
#11638=DIRECTION('center_axis',(0.,1.,0.));
#11639=DIRECTION('ref_axis',(0.,0.,1.));
#11640=DIRECTION('center_axis',(0.,-1.,0.));
#11641=DIRECTION('ref_axis',(0.,0.,-1.));
#11642=DIRECTION('center_axis',(0.,-1.,0.));
#11643=DIRECTION('ref_axis',(0.,0.,-1.));
#11644=DIRECTION('',(-1.,0.,0.));
#11645=DIRECTION('center_axis',(0.,1.,0.));
#11646=DIRECTION('ref_axis',(0.,0.,1.));
#11647=DIRECTION('center_axis',(0.,0.,1.));
#11648=DIRECTION('ref_axis',(1.,0.,0.));
#11649=DIRECTION('center_axis',(0.,1.,0.));
#11650=DIRECTION('ref_axis',(0.,0.,1.));
#11651=DIRECTION('center_axis',(0.,-1.,0.));
#11652=DIRECTION('ref_axis',(0.,0.,-1.));
#11653=DIRECTION('axis',(0.,0.,1.));
#11654=DIRECTION('refdir',(1.,0.,0.));
#11655=DIRECTION('center_axis',(0.,0.,-1.));
#11656=DIRECTION('ref_axis',(-1.,0.,0.));
#11657=DIRECTION('center_axis',(0.,0.,1.));
#11658=DIRECTION('ref_axis',(1.,0.,0.));
#11659=DIRECTION('',(0.,0.,-1.));
#11660=DIRECTION('center_axis',(0.,0.,1.));
#11661=DIRECTION('ref_axis',(-1.,0.,0.));
#11662=DIRECTION('center_axis',(0.,0.,-1.));
#11663=DIRECTION('ref_axis',(-1.,0.,0.));
#11664=DIRECTION('center_axis',(0.,0.,1.));
#11665=DIRECTION('ref_axis',(1.,0.,0.));
#11666=DIRECTION('',(0.,0.,-1.));
#11667=DIRECTION('center_axis',(0.,0.,1.));
#11668=DIRECTION('ref_axis',(-1.,0.,0.));
#11669=DIRECTION('center_axis',(0.,-1.,0.));
#11670=DIRECTION('ref_axis',(0.,0.,-1.));
#11671=DIRECTION('center_axis',(0.,1.,0.));
#11672=DIRECTION('ref_axis',(0.,0.,-1.));
#11673=DIRECTION('',(0.,-1.,0.));
#11674=DIRECTION('center_axis',(0.,1.,0.));
#11675=DIRECTION('ref_axis',(0.,0.,1.));
#11676=DIRECTION('center_axis',(0.,-1.,0.));
#11677=DIRECTION('ref_axis',(0.,0.,-1.));
#11678=DIRECTION('center_axis',(0.,1.,0.));
#11679=DIRECTION('ref_axis',(0.,0.,-1.));
#11680=DIRECTION('',(0.,-1.,0.));
#11681=DIRECTION('center_axis',(0.,1.,0.));
#11682=DIRECTION('ref_axis',(0.,0.,1.));
#11683=DIRECTION('center_axis',(0.,-1.,0.));
#11684=DIRECTION('ref_axis',(0.,0.,-1.));
#11685=DIRECTION('center_axis',(0.,1.,0.));
#11686=DIRECTION('ref_axis',(0.,0.,1.));
#11687=DIRECTION('',(0.,-1.,0.));
#11688=DIRECTION('center_axis',(0.,1.,0.));
#11689=DIRECTION('ref_axis',(0.,0.,-1.));
#11690=DIRECTION('center_axis',(0.,0.,1.));
#11691=DIRECTION('ref_axis',(1.,0.,0.));
#11692=DIRECTION('',(0.,-1.,0.));
#11693=DIRECTION('',(-1.,0.,0.));
#11694=DIRECTION('',(0.,-1.,0.));
#11695=DIRECTION('',(-1.,0.,0.));
#11696=DIRECTION('center_axis',(0.,0.,1.));
#11697=DIRECTION('ref_axis',(1.,0.,0.));
#11698=DIRECTION('',(0.,1.,0.));
#11699=DIRECTION('',(-1.,0.,0.));
#11700=DIRECTION('',(0.,-1.,0.));
#11701=DIRECTION('',(-1.,0.,0.));
#11702=DIRECTION('center_axis',(1.,0.,0.));
#11703=DIRECTION('ref_axis',(0.,0.,-1.));
#11704=DIRECTION('',(0.,0.,1.));
#11705=DIRECTION('',(0.,-1.,0.));
#11706=DIRECTION('',(0.,0.,1.));
#11707=DIRECTION('center_axis',(0.70710678118654,0.,-0.707106781186555));
#11708=DIRECTION('ref_axis',(-0.707106781186555,0.,-0.70710678118654));
#11709=DIRECTION('',(0.707106781186555,0.,0.70710678118654));
#11710=DIRECTION('',(0.,-1.,0.));
#11711=DIRECTION('',(0.707106781186555,0.,0.70710678118654));
#11712=DIRECTION('center_axis',(0.,0.,-1.));
#11713=DIRECTION('ref_axis',(-1.,0.,0.));
#11714=DIRECTION('',(1.,0.,0.));
#11715=DIRECTION('',(0.,-1.,0.));
#11716=DIRECTION('',(1.,0.,0.));
#11717=DIRECTION('center_axis',(-0.707106781186565,0.,-0.70710678118653));
#11718=DIRECTION('ref_axis',(-0.70710678118653,0.,0.707106781186565));
#11719=DIRECTION('',(0.70710678118653,0.,-0.707106781186565));
#11720=DIRECTION('',(0.,-1.,0.));
#11721=DIRECTION('',(0.70710678118653,0.,-0.707106781186565));
#11722=DIRECTION('center_axis',(-1.,0.,0.));
#11723=DIRECTION('ref_axis',(0.,0.,1.));
#11724=DIRECTION('',(0.,0.,-1.));
#11725=DIRECTION('',(0.,0.,-1.));
#11726=DIRECTION('center_axis',(0.,-1.,0.));
#11727=DIRECTION('ref_axis',(0.,0.,-1.));
#11728=DIRECTION('',(0.,0.,-1.));
#11729=DIRECTION('',(-1.,0.,0.));
#11730=DIRECTION('',(0.,0.,-1.));
#11731=DIRECTION('center_axis',(0.,-1.,0.));
#11732=DIRECTION('ref_axis',(0.,0.,-1.));
#11733=DIRECTION('',(0.,0.,-1.));
#11734=DIRECTION('',(1.,0.,0.));
#11735=DIRECTION('',(0.,0.,-1.));
#11736=DIRECTION('center_axis',(-1.,0.,0.));
#11737=DIRECTION('ref_axis',(0.,0.,1.));
#11738=DIRECTION('',(0.,1.,0.));
#11739=DIRECTION('center_axis',(1.,0.,0.));
#11740=DIRECTION('ref_axis',(0.,0.,-1.));
#11741=DIRECTION('',(0.,-1.,0.));
#11742=DIRECTION('center_axis',(0.,0.,-1.));
#11743=DIRECTION('ref_axis',(-1.,0.,0.));
#11744=DIRECTION('center_axis',(0.,1.,0.));
#11745=DIRECTION('ref_axis',(0.,0.,1.));
#11746=DIRECTION('center_axis',(0.,1.,0.));
#11747=DIRECTION('ref_axis',(0.,0.,1.));
#11748=DIRECTION('center_axis',(0.,1.,0.));
#11749=DIRECTION('ref_axis',(0.,0.,1.));
#11750=DIRECTION('center_axis',(0.,0.,1.));
#11751=DIRECTION('ref_axis',(1.,0.,0.));
#11752=DIRECTION('center_axis',(0.,0.,1.));
#11753=DIRECTION('ref_axis',(1.,0.,0.));
#11754=DIRECTION('axis',(0.,0.,1.));
#11755=DIRECTION('refdir',(1.,0.,0.));
#11756=DIRECTION('center_axis',(0.,0.83205103426688,-0.55469908633007));
#11757=DIRECTION('ref_axis',(0.,0.55469908633007,0.83205103426688));
#11758=DIRECTION('',(0.,-0.55469908633007,-0.83205103426688));
#11759=DIRECTION('',(-1.,0.,0.));
#11760=DIRECTION('',(0.,-0.55469908633007,-0.83205103426688));
#11761=DIRECTION('',(-1.,0.,0.));
#11762=DIRECTION('center_axis',(0.,0.,1.));
#11763=DIRECTION('ref_axis',(1.,0.,0.));
#11764=DIRECTION('',(0.,1.,0.));
#11765=DIRECTION('',(-1.,0.,0.));
#11766=DIRECTION('',(0.,1.,0.));
#11767=DIRECTION('center_axis',(0.,-0.83205103426688,0.55469908633007));
#11768=DIRECTION('ref_axis',(0.,-0.55469908633007,-0.83205103426688));
#11769=DIRECTION('',(0.,0.55469908633007,0.83205103426688));
#11770=DIRECTION('',(-1.,0.,0.));
#11771=DIRECTION('',(0.,0.55469908633007,0.83205103426688));
#11772=DIRECTION('center_axis',(0.,0.,-1.));
#11773=DIRECTION('ref_axis',(-1.,0.,0.));
#11774=DIRECTION('',(0.,-1.,0.));
#11775=DIRECTION('',(0.,-1.,0.));
#11776=DIRECTION('center_axis',(1.,0.,0.));
#11777=DIRECTION('ref_axis',(0.,0.,-1.));
#11778=DIRECTION('center_axis',(1.,0.,0.));
#11779=DIRECTION('ref_axis',(0.,0.,-1.));
#11780=DIRECTION('axis',(0.,0.,1.));
#11781=DIRECTION('refdir',(1.,0.,0.));
#11782=DIRECTION('center_axis',(0.83205103426688,0.,-0.55469908633007));
#11783=DIRECTION('ref_axis',(-0.55469908633007,0.,-0.83205103426688));
#11784=DIRECTION('',(0.55469908633007,0.,0.832051034266881));
#11785=DIRECTION('',(0.,-1.,0.));
#11786=DIRECTION('',(0.55469908633007,0.,0.832051034266881));
#11787=DIRECTION('',(0.,-1.,0.));
#11788=DIRECTION('center_axis',(0.,0.,-1.));
#11789=DIRECTION('ref_axis',(-1.,0.,0.));
#11790=DIRECTION('',(1.,0.,0.));
#11791=DIRECTION('',(0.,-1.,0.));
#11792=DIRECTION('',(1.,0.,0.));
#11793=DIRECTION('center_axis',(-0.83205103426688,0.,0.55469908633007));
#11794=DIRECTION('ref_axis',(0.55469908633007,0.,0.83205103426688));
#11795=DIRECTION('',(-0.55469908633007,0.,-0.832051034266881));
#11796=DIRECTION('',(0.,-1.,0.));
#11797=DIRECTION('',(-0.55469908633007,0.,-0.832051034266881));
#11798=DIRECTION('center_axis',(0.,0.,1.));
#11799=DIRECTION('ref_axis',(1.,0.,0.));
#11800=DIRECTION('',(-1.,0.,0.));
#11801=DIRECTION('',(-1.,0.,0.));
#11802=DIRECTION('center_axis',(0.,-1.,0.));
#11803=DIRECTION('ref_axis',(0.,0.,-1.));
#11804=DIRECTION('center_axis',(0.,-1.,0.));
#11805=DIRECTION('ref_axis',(0.,0.,-1.));
#11806=DIRECTION('axis',(0.,0.,1.));
#11807=DIRECTION('refdir',(1.,0.,0.));
#11808=DIRECTION('center_axis',(0.,0.,-1.));
#11809=DIRECTION('ref_axis',(-1.,0.,0.));
#11810=DIRECTION('center_axis',(0.,0.,1.));
#11811=DIRECTION('ref_axis',(1.,0.,0.));
#11812=DIRECTION('',(0.,0.,-1.));
#11813=DIRECTION('center_axis',(0.,0.,1.));
#11814=DIRECTION('ref_axis',(-1.,0.,0.));
#11815=DIRECTION('center_axis',(0.,0.,-1.));
#11816=DIRECTION('ref_axis',(-1.,0.,0.));
#11817=DIRECTION('center_axis',(0.,0.,1.));
#11818=DIRECTION('ref_axis',(1.,0.,0.));
#11819=DIRECTION('',(0.,0.,-1.));
#11820=DIRECTION('center_axis',(0.,0.,1.));
#11821=DIRECTION('ref_axis',(-1.,0.,0.));
#11822=DIRECTION('center_axis',(0.,0.,-1.));
#11823=DIRECTION('ref_axis',(-1.,0.,0.));
#11824=DIRECTION('center_axis',(0.,0.,1.));
#11825=DIRECTION('ref_axis',(-1.,0.,0.));
#11826=DIRECTION('',(0.,0.,-1.));
#11827=DIRECTION('center_axis',(0.,0.,1.));
#11828=DIRECTION('ref_axis',(1.,0.,0.));
#11829=DIRECTION('center_axis',(0.,0.,-1.));
#11830=DIRECTION('ref_axis',(-1.,0.,0.));
#11831=DIRECTION('center_axis',(0.,0.,1.));
#11832=DIRECTION('ref_axis',(-1.,0.,0.));
#11833=DIRECTION('',(0.,0.,-1.));
#11834=DIRECTION('center_axis',(0.,0.,1.));
#11835=DIRECTION('ref_axis',(1.,0.,0.));
#11836=DIRECTION('center_axis',(-1.,0.,0.));
#11837=DIRECTION('ref_axis',(0.,0.,1.));
#11838=DIRECTION('',(0.,1.,0.));
#11839=DIRECTION('',(0.,0.,-1.));
#11840=DIRECTION('',(0.,1.,0.));
#11841=DIRECTION('',(0.,0.,-1.));
#11842=DIRECTION('center_axis',(0.,-1.,0.));
#11843=DIRECTION('ref_axis',(0.,0.,-1.));
#11844=DIRECTION('',(-1.,0.,0.));
#11845=DIRECTION('',(0.,0.,-1.));
#11846=DIRECTION('',(-1.,0.,0.));
#11847=DIRECTION('center_axis',(1.,0.,0.));
#11848=DIRECTION('ref_axis',(0.,0.,-1.));
#11849=DIRECTION('',(0.,-1.,0.));
#11850=DIRECTION('',(0.,0.,-1.));
#11851=DIRECTION('',(0.,-1.,0.));
#11852=DIRECTION('center_axis',(0.,1.,0.));
#11853=DIRECTION('ref_axis',(0.,0.,1.));
#11854=DIRECTION('',(1.,0.,0.));
#11855=DIRECTION('',(1.,0.,0.));
#11856=DIRECTION('center_axis',(0.,0.,-1.));
#11857=DIRECTION('ref_axis',(-1.,0.,0.));
#11858=DIRECTION('center_axis',(0.,0.,-1.));
#11859=DIRECTION('ref_axis',(-1.,0.,0.));
#11860=DIRECTION('center_axis',(0.,0.,1.));
#11861=DIRECTION('ref_axis',(1.,0.,0.));
#11862=DIRECTION('center_axis',(0.,0.,1.));
#11863=DIRECTION('ref_axis',(1.,0.,0.));
#11864=DIRECTION('axis',(0.,0.,1.));
#11865=DIRECTION('refdir',(1.,0.,0.));
#11866=DIRECTION('center_axis',(0.,0.,-1.));
#11867=DIRECTION('ref_axis',(-1.,0.,0.));
#11868=DIRECTION('center_axis',(0.,0.,-1.));
#11869=DIRECTION('ref_axis',(-1.,0.,0.));
#11870=DIRECTION('',(0.,0.,1.));
#11871=DIRECTION('center_axis',(0.,0.,-1.));
#11872=DIRECTION('ref_axis',(-1.,0.,0.));
#11873=DIRECTION('center_axis',(0.,0.,-1.));
#11874=DIRECTION('ref_axis',(-1.,0.,0.));
#11875=DIRECTION('center_axis',(0.,0.,-1.));
#11876=DIRECTION('ref_axis',(-1.,0.,0.));
#11877=DIRECTION('',(0.,0.,1.));
#11878=DIRECTION('center_axis',(0.,0.,-1.));
#11879=DIRECTION('ref_axis',(-1.,0.,0.));
#11880=DIRECTION('center_axis',(0.,0.,-1.));
#11881=DIRECTION('ref_axis',(-1.,0.,0.));
#11882=DIRECTION('center_axis',(0.,0.,-1.));
#11883=DIRECTION('ref_axis',(-1.,0.,0.));
#11884=DIRECTION('',(0.,0.,1.));
#11885=DIRECTION('center_axis',(0.,0.,-1.));
#11886=DIRECTION('ref_axis',(-1.,0.,0.));
#11887=DIRECTION('center_axis',(0.,0.,-1.));
#11888=DIRECTION('ref_axis',(-1.,0.,0.));
#11889=DIRECTION('center_axis',(0.,0.,-1.));
#11890=DIRECTION('ref_axis',(-1.,0.,0.));
#11891=DIRECTION('',(0.,0.,1.));
#11892=DIRECTION('center_axis',(0.,0.,-1.));
#11893=DIRECTION('ref_axis',(-1.,0.,0.));
#11894=DIRECTION('center_axis',(0.,0.,-1.));
#11895=DIRECTION('ref_axis',(-1.,0.,0.));
#11896=DIRECTION('center_axis',(0.,0.,-1.));
#11897=DIRECTION('ref_axis',(-1.,0.,0.));
#11898=DIRECTION('',(0.,0.,1.));
#11899=DIRECTION('center_axis',(0.,0.,-1.));
#11900=DIRECTION('ref_axis',(-1.,0.,0.));
#11901=DIRECTION('center_axis',(0.,0.,1.));
#11902=DIRECTION('ref_axis',(1.,0.,0.));
#11903=DIRECTION('center_axis',(0.,0.,1.));
#11904=DIRECTION('ref_axis',(1.,0.,0.));
#11905=DIRECTION('center_axis',(0.,0.,1.));
#11906=DIRECTION('ref_axis',(1.,0.,0.));
#11907=DIRECTION('center_axis',(0.,0.,-1.));
#11908=DIRECTION('ref_axis',(-1.,0.,0.));
#11909=DIRECTION('center_axis',(0.,0.,-1.));
#11910=DIRECTION('ref_axis',(-1.,0.,0.));
#11911=DIRECTION('center_axis',(0.,0.,-1.));
#11912=DIRECTION('ref_axis',(-1.,0.,0.));
#11913=DIRECTION('axis',(0.,0.,1.));
#11914=DIRECTION('refdir',(1.,0.,0.));
#11915=DIRECTION('center_axis',(0.,0.,-1.));
#11916=DIRECTION('ref_axis',(-1.,0.,0.));
#11917=DIRECTION('center_axis',(0.,0.,-1.));
#11918=DIRECTION('ref_axis',(-1.,0.,0.));
#11919=DIRECTION('',(0.,0.,1.));
#11920=DIRECTION('center_axis',(0.,0.,-1.));
#11921=DIRECTION('ref_axis',(-1.,0.,0.));
#11922=DIRECTION('center_axis',(0.,0.,-1.));
#11923=DIRECTION('ref_axis',(-1.,0.,0.));
#11924=DIRECTION('center_axis',(0.,0.,-1.));
#11925=DIRECTION('ref_axis',(-1.,0.,0.));
#11926=DIRECTION('',(0.,0.,1.));
#11927=DIRECTION('center_axis',(0.,0.,-1.));
#11928=DIRECTION('ref_axis',(-1.,0.,0.));
#11929=DIRECTION('center_axis',(0.,0.,-1.));
#11930=DIRECTION('ref_axis',(-1.,0.,0.));
#11931=DIRECTION('center_axis',(0.,0.,-1.));
#11932=DIRECTION('ref_axis',(-1.,0.,0.));
#11933=DIRECTION('',(0.,0.,1.));
#11934=DIRECTION('center_axis',(0.,0.,-1.));
#11935=DIRECTION('ref_axis',(-1.,0.,0.));
#11936=DIRECTION('center_axis',(0.,0.,-1.));
#11937=DIRECTION('ref_axis',(-1.,0.,0.));
#11938=DIRECTION('center_axis',(0.,0.,-1.));
#11939=DIRECTION('ref_axis',(-1.,0.,0.));
#11940=DIRECTION('',(0.,0.,1.));
#11941=DIRECTION('center_axis',(0.,0.,-1.));
#11942=DIRECTION('ref_axis',(-1.,0.,0.));
#11943=DIRECTION('center_axis',(0.,0.,-1.));
#11944=DIRECTION('ref_axis',(-1.,0.,0.));
#11945=DIRECTION('center_axis',(0.,0.,-1.));
#11946=DIRECTION('ref_axis',(-1.,0.,0.));
#11947=DIRECTION('',(0.,0.,1.));
#11948=DIRECTION('center_axis',(0.,0.,-1.));
#11949=DIRECTION('ref_axis',(-1.,0.,0.));
#11950=DIRECTION('center_axis',(0.,0.,1.));
#11951=DIRECTION('ref_axis',(1.,0.,0.));
#11952=DIRECTION('center_axis',(0.,0.,1.));
#11953=DIRECTION('ref_axis',(1.,0.,0.));
#11954=DIRECTION('center_axis',(0.,0.,1.));
#11955=DIRECTION('ref_axis',(1.,0.,0.));
#11956=DIRECTION('center_axis',(0.,0.,-1.));
#11957=DIRECTION('ref_axis',(-1.,0.,0.));
#11958=DIRECTION('center_axis',(0.,0.,1.));
#11959=DIRECTION('ref_axis',(1.,0.,0.));
#11960=DIRECTION('center_axis',(0.,0.,-1.));
#11961=DIRECTION('ref_axis',(-1.,0.,0.));
#11962=DIRECTION('axis',(0.,0.,1.));
#11963=DIRECTION('refdir',(1.,0.,0.));
#11964=DIRECTION('center_axis',(-1.,0.,0.));
#11965=DIRECTION('ref_axis',(0.,0.,1.));
#11966=DIRECTION('center_axis',(-1.,0.,0.));
#11967=DIRECTION('ref_axis',(0.,0.,-1.));
#11968=DIRECTION('',(-1.,0.,0.));
#11969=DIRECTION('center_axis',(-1.,0.,0.));
#11970=DIRECTION('ref_axis',(0.,0.,1.));
#11971=DIRECTION('',(-1.,0.,0.));
#11972=DIRECTION('center_axis',(1.,0.,0.));
#11973=DIRECTION('ref_axis',(0.,0.,1.));
#11974=DIRECTION('center_axis',(0.,0.,-1.));
#11975=DIRECTION('ref_axis',(-1.,0.,0.));
#11976=DIRECTION('center_axis',(0.,0.,-1.));
#11977=DIRECTION('ref_axis',(-1.,0.,0.));
#11978=DIRECTION('',(0.,0.,1.));
#11979=DIRECTION('center_axis',(0.,0.,-1.));
#11980=DIRECTION('ref_axis',(-1.,0.,0.));
#11981=DIRECTION('center_axis',(0.,0.,-1.));
#11982=DIRECTION('ref_axis',(-1.,0.,0.));
#11983=DIRECTION('center_axis',(0.,0.,-1.));
#11984=DIRECTION('ref_axis',(-1.,0.,0.));
#11985=DIRECTION('',(0.,0.,1.));
#11986=DIRECTION('center_axis',(0.,0.,-1.));
#11987=DIRECTION('ref_axis',(-1.,0.,0.));
#11988=DIRECTION('center_axis',(0.,0.,-1.));
#11989=DIRECTION('ref_axis',(-1.,0.,0.));
#11990=DIRECTION('center_axis',(0.,0.,-1.));
#11991=DIRECTION('ref_axis',(-1.,0.,0.));
#11992=DIRECTION('',(0.,0.,-1.));
#11993=DIRECTION('center_axis',(0.,0.,1.));
#11994=DIRECTION('ref_axis',(1.,0.,0.));
#11995=DIRECTION('',(0.,0.,1.));
#11996=DIRECTION('center_axis',(0.,0.,-1.));
#11997=DIRECTION('ref_axis',(-1.,0.,0.));
#11998=DIRECTION('',(0.,0.,1.));
#11999=DIRECTION('',(0.,0.,1.));
#12000=DIRECTION('center_axis',(0.,0.,-1.));
#12001=DIRECTION('ref_axis',(-1.,0.,0.));
#12002=DIRECTION('center_axis',(0.,0.,-1.));
#12003=DIRECTION('ref_axis',(-1.,0.,0.));
#12004=DIRECTION('',(0.,0.,-1.));
#12005=DIRECTION('center_axis',(0.,0.,1.));
#12006=DIRECTION('ref_axis',(1.,0.,0.));
#12007=DIRECTION('',(0.,0.,1.));
#12008=DIRECTION('center_axis',(0.,0.,1.));
#12009=DIRECTION('ref_axis',(1.,0.,0.));
#12010=DIRECTION('',(0.,1.,0.));
#12011=DIRECTION('center_axis',(0.,0.,1.));
#12012=DIRECTION('ref_axis',(1.,0.,0.));
#12013=DIRECTION('',(0.,-1.,0.));
#12014=DIRECTION('center_axis',(0.,0.,-1.));
#12015=DIRECTION('ref_axis',(-1.,0.,0.));
#12016=DIRECTION('center_axis',(0.,0.,-1.));
#12017=DIRECTION('ref_axis',(-1.,0.,0.));
#12018=DIRECTION('center_axis',(0.,0.,-1.));
#12019=DIRECTION('ref_axis',(-1.,0.,0.));
#12020=DIRECTION('center_axis',(1.,0.,0.));
#12021=DIRECTION('ref_axis',(0.,0.,-1.));
#12022=DIRECTION('',(0.,-1.,0.));
#12023=DIRECTION('center_axis',(-1.,0.,0.));
#12024=DIRECTION('ref_axis',(0.,0.,1.));
#12025=DIRECTION('',(0.,1.,0.));
#12026=DIRECTION('center_axis',(0.,0.,1.));
#12027=DIRECTION('ref_axis',(1.,0.,0.));
#12028=DIRECTION('axis',(0.,0.,1.));
#12029=DIRECTION('refdir',(1.,0.,0.));
#12030=DIRECTION('center_axis',(-1.,0.,0.));
#12031=DIRECTION('ref_axis',(0.,0.,1.));
#12032=DIRECTION('center_axis',(1.,0.,0.));
#12033=DIRECTION('ref_axis',(0.,0.,-1.));
#12034=DIRECTION('',(-1.,0.,0.));
#12035=DIRECTION('center_axis',(1.,0.,0.));
#12036=DIRECTION('ref_axis',(0.,0.,-1.));
#12037=DIRECTION('center_axis',(1.,0.,0.));
#12038=DIRECTION('ref_axis',(0.,0.,-1.));
#12039=DIRECTION('',(0.,-1.,0.));
#12040=DIRECTION('',(0.,0.,-1.));
#12041=DIRECTION('',(0.,1.,0.));
#12042=DIRECTION('',(0.,0.,1.));
#12043=DIRECTION('center_axis',(1.,0.,0.));
#12044=DIRECTION('ref_axis',(0.,0.,-1.));
#12045=DIRECTION('',(0.,-1.,0.));
#12046=DIRECTION('',(0.,0.,1.));
#12047=DIRECTION('',(0.,1.,0.));
#12048=DIRECTION('',(0.,0.,-1.));
#12049=DIRECTION('center_axis',(0.,0.,-1.));
#12050=DIRECTION('ref_axis',(-1.,0.,0.));
#12051=DIRECTION('',(-1.,0.,0.));
#12052=DIRECTION('',(-1.,0.,0.));
#12053=DIRECTION('center_axis',(0.,1.,0.));
#12054=DIRECTION('ref_axis',(0.,0.,1.));
#12055=DIRECTION('',(-1.,0.,0.));
#12056=DIRECTION('center_axis',(0.,0.,1.));
#12057=DIRECTION('ref_axis',(1.,0.,0.));
#12058=DIRECTION('',(-1.,0.,0.));
#12059=DIRECTION('center_axis',(0.,-1.,0.));
#12060=DIRECTION('ref_axis',(0.,0.,-1.));
#12061=DIRECTION('axis',(0.,0.,1.));
#12062=DIRECTION('refdir',(1.,0.,0.));
#12063=DIRECTION('center_axis',(0.,-1.,0.));
#12064=DIRECTION('ref_axis',(0.,0.,-1.));
#12065=DIRECTION('center_axis',(0.,1.,0.));
#12066=DIRECTION('ref_axis',(0.,0.,1.));
#12067=DIRECTION('',(0.,-1.,0.));
#12068=DIRECTION('center_axis',(0.,1.,0.));
#12069=DIRECTION('ref_axis',(0.,0.,1.));
#12070=DIRECTION('center_axis',(0.,1.,0.));
#12071=DIRECTION('ref_axis',(0.,0.,1.));
#12072=DIRECTION('',(0.,0.,-1.));
#12073=DIRECTION('',(-1.,0.,0.));
#12074=DIRECTION('',(0.,0.,1.));
#12075=DIRECTION('',(1.,0.,0.));
#12076=DIRECTION('center_axis',(0.,1.,0.));
#12077=DIRECTION('ref_axis',(0.,0.,1.));
#12078=DIRECTION('',(0.,0.,-1.));
#12079=DIRECTION('',(1.,0.,0.));
#12080=DIRECTION('',(0.,0.,1.));
#12081=DIRECTION('',(-1.,0.,0.));
#12082=DIRECTION('center_axis',(-1.,0.,0.));
#12083=DIRECTION('ref_axis',(0.,0.,1.));
#12084=DIRECTION('',(0.,-1.,0.));
#12085=DIRECTION('',(0.,-1.,0.));
#12086=DIRECTION('center_axis',(0.,0.,1.));
#12087=DIRECTION('ref_axis',(1.,0.,0.));
#12088=DIRECTION('',(0.,-1.,0.));
#12089=DIRECTION('center_axis',(1.,0.,0.));
#12090=DIRECTION('ref_axis',(0.,0.,-1.));
#12091=DIRECTION('',(0.,-1.,0.));
#12092=DIRECTION('center_axis',(0.,0.,-1.));
#12093=DIRECTION('ref_axis',(-1.,0.,0.));
#12094=DIRECTION('axis',(0.,0.,1.));
#12095=DIRECTION('refdir',(1.,0.,0.));
#12096=DIRECTION('center_axis',(-1.,0.,0.));
#12097=DIRECTION('ref_axis',(0.,0.,1.));
#12098=DIRECTION('center_axis',(-1.,0.,0.));
#12099=DIRECTION('ref_axis',(0.,0.,-1.));
#12100=DIRECTION('',(-1.,0.,0.));
#12101=DIRECTION('center_axis',(-1.,0.,0.));
#12102=DIRECTION('ref_axis',(0.,0.,-1.));
#12103=DIRECTION('center_axis',(-1.,0.,0.));
#12104=DIRECTION('ref_axis',(0.,0.,1.));
#12105=DIRECTION('center_axis',(1.,0.,0.));
#12106=DIRECTION('ref_axis',(0.,0.,-1.));
#12107=DIRECTION('center_axis',(1.,0.,0.));
#12108=DIRECTION('ref_axis',(0.,0.,-1.));
#12109=DIRECTION('center_axis',(0.,0.,-1.));
#12110=DIRECTION('ref_axis',(-1.,0.,0.));
#12111=DIRECTION('center_axis',(0.,0.,1.));
#12112=DIRECTION('ref_axis',(1.,0.,0.));
#12113=DIRECTION('',(0.,0.,1.));
#12114=DIRECTION('center_axis',(0.,0.,1.));
#12115=DIRECTION('ref_axis',(1.,0.,0.));
#12116=DIRECTION('center_axis',(0.,0.,-1.));
#12117=DIRECTION('ref_axis',(-1.,0.,0.));
#12118=DIRECTION('center_axis',(0.,0.,1.));
#12119=DIRECTION('ref_axis',(1.,0.,0.));
#12120=DIRECTION('',(0.,0.,1.));
#12121=DIRECTION('center_axis',(0.,0.,1.));
#12122=DIRECTION('ref_axis',(1.,0.,0.));
#12123=DIRECTION('center_axis',(0.,0.,1.));
#12124=DIRECTION('ref_axis',(1.,0.,0.));
#12125=DIRECTION('center_axis',(1.,0.,0.));
#12126=DIRECTION('ref_axis',(0.,0.,-1.));
#12127=DIRECTION('center_axis',(1.,0.,0.));
#12128=DIRECTION('ref_axis',(0.,0.,-1.));
#12129=DIRECTION('axis',(0.,0.,1.));
#12130=DIRECTION('refdir',(1.,0.,0.));
#12131=DIRECTION('center_axis',(0.,0.,-1.));
#12132=DIRECTION('ref_axis',(-1.,0.,0.));
#12133=DIRECTION('center_axis',(0.,0.,1.));
#12134=DIRECTION('ref_axis',(1.,0.,0.));
#12135=DIRECTION('',(0.,0.,1.));
#12136=DIRECTION('center_axis',(0.,0.,1.));
#12137=DIRECTION('ref_axis',(1.,0.,0.));
#12138=DIRECTION('center_axis',(0.,0.,1.));
#12139=DIRECTION('ref_axis',(1.,0.,0.));
#12140=DIRECTION('center_axis',(0.,0.,1.));
#12141=DIRECTION('ref_axis',(1.,0.,0.));
#12142=DIRECTION('axis',(0.,0.,1.));
#12143=DIRECTION('refdir',(1.,0.,0.));
#12144=DIRECTION('center_axis',(0.,-1.,0.));
#12145=DIRECTION('ref_axis',(0.,0.,-1.));
#12146=DIRECTION('center_axis',(0.,1.,0.));
#12147=DIRECTION('ref_axis',(0.,0.,1.));
#12148=DIRECTION('',(0.,-1.,0.));
#12149=DIRECTION('center_axis',(0.,1.,0.));
#12150=DIRECTION('ref_axis',(0.,0.,1.));
#12151=DIRECTION('center_axis',(0.,-1.,0.));
#12152=DIRECTION('ref_axis',(0.,0.,-1.));
#12153=DIRECTION('center_axis',(0.,1.,0.));
#12154=DIRECTION('ref_axis',(0.,0.,1.));
#12155=DIRECTION('',(0.,-1.,0.));
#12156=DIRECTION('center_axis',(0.,1.,0.));
#12157=DIRECTION('ref_axis',(0.,0.,1.));
#12158=DIRECTION('center_axis',(0.,-1.,0.));
#12159=DIRECTION('ref_axis',(0.,0.,-1.));
#12160=DIRECTION('center_axis',(0.,-1.,0.));
#12161=DIRECTION('ref_axis',(0.,0.,1.));
#12162=DIRECTION('',(0.,-1.,0.));
#12163=DIRECTION('center_axis',(0.,1.,0.));
#12164=DIRECTION('ref_axis',(0.,0.,1.));
#12165=DIRECTION('center_axis',(0.,-1.,0.));
#12166=DIRECTION('ref_axis',(0.,0.,-1.));
#12167=DIRECTION('center_axis',(0.,-1.,0.));
#12168=DIRECTION('ref_axis',(0.,0.,1.));
#12169=DIRECTION('',(0.,-1.,0.));
#12170=DIRECTION('center_axis',(0.,1.,0.));
#12171=DIRECTION('ref_axis',(0.,0.,1.));
#12172=DIRECTION('center_axis',(-1.,0.,0.));
#12173=DIRECTION('ref_axis',(0.,0.,1.));
#12174=DIRECTION('',(0.,0.,-1.));
#12175=DIRECTION('',(0.,-1.,0.));
#12176=DIRECTION('',(0.,0.,-1.));
#12177=DIRECTION('',(0.,-1.,0.));
#12178=DIRECTION('center_axis',(0.,0.,1.));
#12179=DIRECTION('ref_axis',(1.,0.,0.));
#12180=DIRECTION('',(-1.,0.,0.));
#12181=DIRECTION('',(0.,-1.,0.));
#12182=DIRECTION('',(-1.,0.,0.));
#12183=DIRECTION('center_axis',(1.,0.,0.));
#12184=DIRECTION('ref_axis',(0.,0.,-1.));
#12185=DIRECTION('',(0.,0.,1.));
#12186=DIRECTION('',(0.,-1.,0.));
#12187=DIRECTION('',(0.,0.,1.));
#12188=DIRECTION('center_axis',(0.,0.,-1.));
#12189=DIRECTION('ref_axis',(-1.,0.,0.));
#12190=DIRECTION('',(1.,0.,0.));
#12191=DIRECTION('',(1.,0.,0.));
#12192=DIRECTION('center_axis',(0.,1.,0.));
#12193=DIRECTION('ref_axis',(0.,0.,1.));
#12194=DIRECTION('center_axis',(0.,1.,0.));
#12195=DIRECTION('ref_axis',(0.,0.,1.));
#12196=DIRECTION('center_axis',(0.,1.,0.));
#12197=DIRECTION('ref_axis',(0.,0.,1.));
#12198=DIRECTION('center_axis',(0.,1.,0.));
#12199=DIRECTION('ref_axis',(0.,0.,1.));
#12200=DIRECTION('axis',(0.,0.,1.));
#12201=DIRECTION('refdir',(1.,0.,0.));
#12202=DIRECTION('center_axis',(0.,0.,-1.));
#12203=DIRECTION('ref_axis',(-1.,0.,0.));
#12204=DIRECTION('center_axis',(0.,0.,1.));
#12205=DIRECTION('ref_axis',(1.,0.,0.));
#12206=DIRECTION('',(0.,0.,-1.));
#12207=DIRECTION('center_axis',(0.,0.,1.));
#12208=DIRECTION('ref_axis',(1.,0.,0.));
#12209=DIRECTION('center_axis',(0.,0.,-1.));
#12210=DIRECTION('ref_axis',(-1.,0.,0.));
#12211=DIRECTION('center_axis',(0.,0.,1.));
#12212=DIRECTION('ref_axis',(1.,0.,0.));
#12213=DIRECTION('',(0.,0.,-1.));
#12214=DIRECTION('center_axis',(0.,0.,1.));
#12215=DIRECTION('ref_axis',(1.,0.,0.));
#12216=DIRECTION('center_axis',(0.,0.,-1.));
#12217=DIRECTION('ref_axis',(-1.,0.,0.));
#12218=DIRECTION('center_axis',(0.,0.,1.));
#12219=DIRECTION('ref_axis',(1.,0.,0.));
#12220=DIRECTION('',(0.,0.,-1.));
#12221=DIRECTION('center_axis',(0.,0.,1.));
#12222=DIRECTION('ref_axis',(1.,0.,0.));
#12223=DIRECTION('center_axis',(0.,0.,1.));
#12224=DIRECTION('ref_axis',(1.,0.,0.));
#12225=DIRECTION('',(0.,-1.,0.));
#12226=DIRECTION('',(0.707106781186548,-0.707106781186548,0.));
#12227=DIRECTION('',(1.,0.,0.));
#12228=DIRECTION('',(0.707106781186548,0.707106781186548,0.));
#12229=DIRECTION('',(0.,1.,0.));
#12230=DIRECTION('',(-0.707106781186548,0.707106781186548,0.));
#12231=DIRECTION('',(-1.,0.,0.));
#12232=DIRECTION('',(-0.707106781186548,-0.707106781186548,0.));
#12233=DIRECTION('center_axis',(0.,0.,1.));
#12234=DIRECTION('ref_axis',(1.,0.,0.));
#12235=DIRECTION('',(0.,-1.,0.));
#12236=DIRECTION('',(-0.707106781186548,-0.707106781186548,0.));
#12237=DIRECTION('',(-1.,0.,0.));
#12238=DIRECTION('',(-0.707106781186548,0.707106781186548,0.));
#12239=DIRECTION('',(0.,1.,0.));
#12240=DIRECTION('',(0.707106781186548,0.707106781186548,0.));
#12241=DIRECTION('',(1.,0.,0.));
#12242=DIRECTION('',(0.707106781186548,-0.707106781186548,0.));
#12243=DIRECTION('center_axis',(1.,0.,0.));
#12244=DIRECTION('ref_axis',(0.,0.,-1.));
#12245=DIRECTION('',(0.,0.,-1.));
#12246=DIRECTION('',(0.,0.,-1.));
#12247=DIRECTION('center_axis',(0.707106781186548,0.707106781186547,0.));
#12248=DIRECTION('ref_axis',(-0.707106781186547,0.707106781186548,0.));
#12249=DIRECTION('',(0.,0.,-1.));
#12250=DIRECTION('center_axis',(0.,1.,0.));
#12251=DIRECTION('ref_axis',(0.,0.,1.));
#12252=DIRECTION('',(0.,0.,-1.));
#12253=DIRECTION('center_axis',(-0.707106781186548,0.707106781186547,0.));
#12254=DIRECTION('ref_axis',(-0.707106781186547,-0.707106781186548,0.));
#12255=DIRECTION('',(0.,0.,-1.));
#12256=DIRECTION('center_axis',(-1.,0.,0.));
#12257=DIRECTION('ref_axis',(0.,0.,1.));
#12258=DIRECTION('',(0.,0.,-1.));
#12259=DIRECTION('center_axis',(-0.707106781186548,-0.707106781186547,0.));
#12260=DIRECTION('ref_axis',(0.707106781186547,-0.707106781186548,0.));
#12261=DIRECTION('',(0.,0.,-1.));
#12262=DIRECTION('center_axis',(0.,-1.,0.));
#12263=DIRECTION('ref_axis',(0.,0.,-1.));
#12264=DIRECTION('',(0.,0.,-1.));
#12265=DIRECTION('center_axis',(0.707106781186548,-0.707106781186547,0.));
#12266=DIRECTION('ref_axis',(0.707106781186547,0.707106781186548,0.));
#12267=DIRECTION('axis',(0.,0.,1.));
#12268=DIRECTION('refdir',(1.,0.,0.));
#12269=DIRECTION('center_axis',(0.,0.,-1.));
#12270=DIRECTION('ref_axis',(-1.,0.,0.));
#12271=DIRECTION('center_axis',(0.,0.,1.));
#12272=DIRECTION('ref_axis',(1.,0.,0.));
#12273=DIRECTION('',(0.,0.,-1.));
#12274=DIRECTION('center_axis',(0.,0.,1.));
#12275=DIRECTION('ref_axis',(1.,0.,0.));
#12276=DIRECTION('center_axis',(0.,0.,-1.));
#12277=DIRECTION('ref_axis',(-1.,0.,0.));
#12278=DIRECTION('center_axis',(0.,0.,1.));
#12279=DIRECTION('ref_axis',(1.,0.,0.));
#12280=DIRECTION('',(0.,0.,1.));
#12281=DIRECTION('center_axis',(0.,0.,1.));
#12282=DIRECTION('ref_axis',(1.,0.,0.));
#12283=DIRECTION('',(0.,0.,-1.));
#12284=DIRECTION('center_axis',(0.,0.,1.));
#12285=DIRECTION('ref_axis',(1.,0.,0.));
#12286=DIRECTION('',(0.,0.,1.));
#12287=DIRECTION('center_axis',(0.,0.,1.));
#12288=DIRECTION('ref_axis',(1.,0.,0.));
#12289=DIRECTION('center_axis',(0.,0.,1.));
#12290=DIRECTION('ref_axis',(1.,0.,0.));
#12291=DIRECTION('',(0.,0.,1.));
#12292=DIRECTION('center_axis',(0.,0.,1.));
#12293=DIRECTION('ref_axis',(1.,0.,0.));
#12294=DIRECTION('center_axis',(0.,0.,1.));
#12295=DIRECTION('ref_axis',(1.,0.,0.));
#12296=DIRECTION('',(0.,0.,1.));
#12297=DIRECTION('center_axis',(0.,0.,1.));
#12298=DIRECTION('ref_axis',(1.,0.,0.));
#12299=DIRECTION('',(0.,0.,-1.));
#12300=DIRECTION('',(0.,0.,-1.));
#12301=DIRECTION('center_axis',(0.,0.,1.));
#12302=DIRECTION('ref_axis',(1.,0.,0.));
#12303=DIRECTION('',(0.,0.,1.));
#12304=DIRECTION('center_axis',(0.,0.,1.));
#12305=DIRECTION('ref_axis',(1.,0.,0.));
#12306=DIRECTION('',(0.,0.,-1.));
#12307=DIRECTION('center_axis',(0.,0.,1.));
#12308=DIRECTION('ref_axis',(1.,0.,0.));
#12309=DIRECTION('',(0.,0.,1.));
#12310=DIRECTION('center_axis',(0.,0.,1.));
#12311=DIRECTION('ref_axis',(1.,0.,0.));
#12312=DIRECTION('',(0.,0.,-1.));
#12313=DIRECTION('center_axis',(0.,0.,1.));
#12314=DIRECTION('ref_axis',(1.,0.,0.));
#12315=DIRECTION('',(0.,0.,1.));
#12316=DIRECTION('center_axis',(0.,0.,1.));
#12317=DIRECTION('ref_axis',(1.,0.,0.));
#12318=DIRECTION('',(0.,0.,-1.));
#12319=DIRECTION('center_axis',(0.,0.,1.));
#12320=DIRECTION('ref_axis',(1.,0.,0.));
#12321=DIRECTION('',(0.,0.,1.));
#12322=DIRECTION('center_axis',(0.,0.,1.));
#12323=DIRECTION('ref_axis',(1.,0.,0.));
#12324=DIRECTION('',(0.,0.,-1.));
#12325=DIRECTION('center_axis',(0.,0.,1.));
#12326=DIRECTION('ref_axis',(1.,0.,0.));
#12327=DIRECTION('',(0.,0.,1.));
#12328=DIRECTION('center_axis',(0.,0.,1.));
#12329=DIRECTION('ref_axis',(1.,0.,0.));
#12330=DIRECTION('',(0.,0.,-1.));
#12331=DIRECTION('center_axis',(0.,0.,1.));
#12332=DIRECTION('ref_axis',(1.,0.,0.));
#12333=DIRECTION('',(0.,0.,1.));
#12334=DIRECTION('center_axis',(0.,0.,1.));
#12335=DIRECTION('ref_axis',(1.,0.,0.));
#12336=DIRECTION('',(0.,0.,-1.));
#12337=DIRECTION('center_axis',(0.,0.,1.));
#12338=DIRECTION('ref_axis',(1.,0.,0.));
#12339=DIRECTION('',(0.,0.,1.));
#12340=DIRECTION('center_axis',(0.,0.,1.));
#12341=DIRECTION('ref_axis',(1.,0.,0.));
#12342=DIRECTION('',(0.,0.,-1.));
#12343=DIRECTION('center_axis',(0.,0.,1.));
#12344=DIRECTION('ref_axis',(1.,0.,0.));
#12345=DIRECTION('',(0.,0.,1.));
#12346=DIRECTION('center_axis',(0.,0.,1.));
#12347=DIRECTION('ref_axis',(1.,0.,0.));
#12348=DIRECTION('',(0.,0.,-1.));
#12349=DIRECTION('center_axis',(0.,0.,1.));
#12350=DIRECTION('ref_axis',(1.,0.,0.));
#12351=DIRECTION('',(0.,0.,1.));
#12352=DIRECTION('center_axis',(0.,0.,1.));
#12353=DIRECTION('ref_axis',(1.,0.,0.));
#12354=DIRECTION('',(0.,0.,-1.));
#12355=DIRECTION('center_axis',(0.,0.,1.));
#12356=DIRECTION('ref_axis',(1.,0.,0.));
#12357=DIRECTION('',(0.,0.,1.));
#12358=DIRECTION('center_axis',(0.,0.,1.));
#12359=DIRECTION('ref_axis',(1.,0.,0.));
#12360=DIRECTION('',(0.,0.,-1.));
#12361=DIRECTION('center_axis',(0.,0.,1.));
#12362=DIRECTION('ref_axis',(1.,0.,0.));
#12363=DIRECTION('',(0.,0.,1.));
#12364=DIRECTION('center_axis',(0.,0.,1.));
#12365=DIRECTION('ref_axis',(1.,0.,0.));
#12366=DIRECTION('',(0.,0.,-1.));
#12367=DIRECTION('center_axis',(0.,0.,1.));
#12368=DIRECTION('ref_axis',(1.,0.,0.));
#12369=DIRECTION('',(0.,0.,1.));
#12370=DIRECTION('center_axis',(0.,0.,1.));
#12371=DIRECTION('ref_axis',(1.,0.,0.));
#12372=DIRECTION('',(0.,0.,-1.));
#12373=DIRECTION('center_axis',(0.,0.,1.));
#12374=DIRECTION('ref_axis',(1.,0.,0.));
#12375=DIRECTION('',(0.,0.,1.));
#12376=DIRECTION('center_axis',(0.,0.,1.));
#12377=DIRECTION('ref_axis',(1.,0.,0.));
#12378=DIRECTION('',(0.,0.,-1.));
#12379=DIRECTION('center_axis',(0.,0.,1.));
#12380=DIRECTION('ref_axis',(1.,0.,0.));
#12381=DIRECTION('',(0.,0.,1.));
#12382=DIRECTION('center_axis',(0.,0.,1.));
#12383=DIRECTION('ref_axis',(1.,0.,0.));
#12384=DIRECTION('',(0.,0.,-1.));
#12385=DIRECTION('center_axis',(0.,0.,1.));
#12386=DIRECTION('ref_axis',(1.,0.,0.));
#12387=DIRECTION('',(0.,0.,1.));
#12388=DIRECTION('center_axis',(0.,0.,1.));
#12389=DIRECTION('ref_axis',(1.,0.,0.));
#12390=DIRECTION('',(0.,0.,-1.));
#12391=DIRECTION('center_axis',(0.,0.,1.));
#12392=DIRECTION('ref_axis',(1.,0.,0.));
#12393=DIRECTION('',(0.,0.,1.));
#12394=DIRECTION('center_axis',(0.,0.,1.));
#12395=DIRECTION('ref_axis',(1.,0.,0.));
#12396=DIRECTION('',(0.,0.,-1.));
#12397=DIRECTION('center_axis',(0.,0.,1.));
#12398=DIRECTION('ref_axis',(1.,0.,0.));
#12399=DIRECTION('',(0.,0.,1.));
#12400=DIRECTION('center_axis',(0.,0.,1.));
#12401=DIRECTION('ref_axis',(1.,0.,0.));
#12402=DIRECTION('',(0.,0.,-1.));
#12403=DIRECTION('center_axis',(0.,0.,1.));
#12404=DIRECTION('ref_axis',(1.,0.,0.));
#12405=DIRECTION('',(0.,0.,1.));
#12406=DIRECTION('center_axis',(0.,0.,1.));
#12407=DIRECTION('ref_axis',(1.,0.,0.));
#12408=DIRECTION('',(0.,0.,-1.));
#12409=DIRECTION('center_axis',(0.,0.,1.));
#12410=DIRECTION('ref_axis',(1.,0.,0.));
#12411=DIRECTION('',(0.,0.,1.));
#12412=DIRECTION('center_axis',(0.,0.,1.));
#12413=DIRECTION('ref_axis',(1.,0.,0.));
#12414=DIRECTION('',(0.,0.,-1.));
#12415=DIRECTION('center_axis',(0.,0.,1.));
#12416=DIRECTION('ref_axis',(1.,0.,0.));
#12417=DIRECTION('',(0.,0.,1.));
#12418=DIRECTION('center_axis',(0.,0.,1.));
#12419=DIRECTION('ref_axis',(1.,0.,0.));
#12420=DIRECTION('',(0.,0.,-1.));
#12421=DIRECTION('center_axis',(0.,0.,1.));
#12422=DIRECTION('ref_axis',(1.,0.,0.));
#12423=DIRECTION('',(0.,0.,1.));
#12424=DIRECTION('center_axis',(0.,0.,1.));
#12425=DIRECTION('ref_axis',(1.,0.,0.));
#12426=DIRECTION('',(0.,0.,-1.));
#12427=DIRECTION('center_axis',(0.,0.,1.));
#12428=DIRECTION('ref_axis',(1.,0.,0.));
#12429=DIRECTION('',(0.,0.,1.));
#12430=DIRECTION('center_axis',(0.,0.,1.));
#12431=DIRECTION('ref_axis',(1.,0.,0.));
#12432=DIRECTION('',(0.,0.,-1.));
#12433=DIRECTION('center_axis',(0.,0.,1.));
#12434=DIRECTION('ref_axis',(1.,0.,0.));
#12435=DIRECTION('',(0.,0.,1.));
#12436=DIRECTION('center_axis',(0.,0.,1.));
#12437=DIRECTION('ref_axis',(1.,0.,0.));
#12438=DIRECTION('',(0.,0.,-1.));
#12439=DIRECTION('center_axis',(0.,0.,1.));
#12440=DIRECTION('ref_axis',(1.,0.,0.));
#12441=DIRECTION('',(0.,0.,1.));
#12442=DIRECTION('center_axis',(0.,0.,1.));
#12443=DIRECTION('ref_axis',(1.,0.,0.));
#12444=DIRECTION('',(0.,0.,-1.));
#12445=DIRECTION('center_axis',(0.,0.,1.));
#12446=DIRECTION('ref_axis',(1.,0.,0.));
#12447=DIRECTION('',(0.,0.,1.));
#12448=DIRECTION('center_axis',(0.,0.,1.));
#12449=DIRECTION('ref_axis',(1.,0.,0.));
#12450=DIRECTION('',(0.,0.,-1.));
#12451=DIRECTION('center_axis',(0.,0.,1.));
#12452=DIRECTION('ref_axis',(1.,0.,0.));
#12453=DIRECTION('',(0.,0.,1.));
#12454=DIRECTION('center_axis',(0.,0.,1.));
#12455=DIRECTION('ref_axis',(1.,0.,0.));
#12456=DIRECTION('',(0.,0.,-1.));
#12457=DIRECTION('center_axis',(0.,0.,1.));
#12458=DIRECTION('ref_axis',(1.,0.,0.));
#12459=DIRECTION('',(0.,0.,1.));
#12460=DIRECTION('center_axis',(0.,0.,1.));
#12461=DIRECTION('ref_axis',(1.,0.,0.));
#12462=DIRECTION('',(0.,0.,-1.));
#12463=DIRECTION('center_axis',(0.,0.,1.));
#12464=DIRECTION('ref_axis',(1.,0.,0.));
#12465=DIRECTION('',(0.,0.,1.));
#12466=DIRECTION('center_axis',(0.,0.,1.));
#12467=DIRECTION('ref_axis',(1.,0.,0.));
#12468=DIRECTION('',(0.,0.,-1.));
#12469=DIRECTION('center_axis',(0.,0.,1.));
#12470=DIRECTION('ref_axis',(1.,0.,0.));
#12471=DIRECTION('',(0.,0.,1.));
#12472=DIRECTION('center_axis',(0.,0.,1.));
#12473=DIRECTION('ref_axis',(1.,0.,0.));
#12474=DIRECTION('',(0.,0.,-1.));
#12475=DIRECTION('center_axis',(0.,0.,1.));
#12476=DIRECTION('ref_axis',(1.,0.,0.));
#12477=DIRECTION('',(0.,0.,1.));
#12478=DIRECTION('center_axis',(0.,0.,1.));
#12479=DIRECTION('ref_axis',(1.,0.,0.));
#12480=DIRECTION('',(0.,0.,-1.));
#12481=DIRECTION('center_axis',(0.,0.,1.));
#12482=DIRECTION('ref_axis',(1.,0.,0.));
#12483=DIRECTION('',(0.,0.,1.));
#12484=DIRECTION('center_axis',(0.,0.,1.));
#12485=DIRECTION('ref_axis',(1.,0.,0.));
#12486=DIRECTION('',(0.,0.,-1.));
#12487=DIRECTION('center_axis',(0.,0.,1.));
#12488=DIRECTION('ref_axis',(1.,0.,0.));
#12489=DIRECTION('',(0.,0.,1.));
#12490=DIRECTION('center_axis',(0.,0.,1.));
#12491=DIRECTION('ref_axis',(1.,0.,0.));
#12492=DIRECTION('',(0.,0.,-1.));
#12493=DIRECTION('center_axis',(0.,0.,1.));
#12494=DIRECTION('ref_axis',(1.,0.,0.));
#12495=DIRECTION('',(0.,0.,1.));
#12496=DIRECTION('center_axis',(0.,0.,1.));
#12497=DIRECTION('ref_axis',(1.,0.,0.));
#12498=DIRECTION('',(0.,0.,-1.));
#12499=DIRECTION('center_axis',(0.,0.,1.));
#12500=DIRECTION('ref_axis',(1.,0.,0.));
#12501=DIRECTION('',(0.,0.,1.));
#12502=DIRECTION('center_axis',(0.,0.,1.));
#12503=DIRECTION('ref_axis',(1.,0.,0.));
#12504=DIRECTION('',(0.,0.,-1.));
#12505=DIRECTION('center_axis',(0.,0.,1.));
#12506=DIRECTION('ref_axis',(1.,0.,0.));
#12507=DIRECTION('',(0.,0.,1.));
#12508=DIRECTION('center_axis',(0.,0.,1.));
#12509=DIRECTION('ref_axis',(1.,0.,0.));
#12510=DIRECTION('',(0.,0.,-1.));
#12511=DIRECTION('center_axis',(0.,0.,1.));
#12512=DIRECTION('ref_axis',(1.,0.,0.));
#12513=DIRECTION('',(0.,0.,1.));
#12514=DIRECTION('center_axis',(0.,0.,1.));
#12515=DIRECTION('ref_axis',(1.,0.,0.));
#12516=DIRECTION('',(0.,0.,-1.));
#12517=DIRECTION('center_axis',(0.,0.,1.));
#12518=DIRECTION('ref_axis',(1.,0.,0.));
#12519=DIRECTION('',(0.,0.,1.));
#12520=DIRECTION('center_axis',(0.,0.,1.));
#12521=DIRECTION('ref_axis',(1.,0.,0.));
#12522=DIRECTION('',(0.,0.,-1.));
#12523=DIRECTION('center_axis',(0.,0.,1.));
#12524=DIRECTION('ref_axis',(1.,0.,0.));
#12525=DIRECTION('',(0.,0.,1.));
#12526=DIRECTION('center_axis',(0.,0.,1.));
#12527=DIRECTION('ref_axis',(1.,0.,0.));
#12528=DIRECTION('center_axis',(0.,0.,1.));
#12529=DIRECTION('ref_axis',(1.,0.,0.));
#12530=DIRECTION('center_axis',(0.,0.,1.));
#12531=DIRECTION('ref_axis',(1.,0.,0.));
#12532=DIRECTION('center_axis',(0.707106781186547,0.707106781186548,0.));
#12533=DIRECTION('ref_axis',(-0.707106781186548,0.707106781186547,0.));
#12534=DIRECTION('',(0.707106781186548,-0.707106781186546,0.));
#12535=DIRECTION('',(0.,0.,-1.));
#12536=DIRECTION('',(0.707106781186548,-0.707106781186546,0.));
#12537=DIRECTION('center_axis',(-0.707106781186548,-0.707106781186547,0.));
#12538=DIRECTION('ref_axis',(0.707106781186547,-0.707106781186548,0.));
#12539=DIRECTION('',(-0.707106781186547,0.707106781186549,0.));
#12540=DIRECTION('',(0.,0.,-1.));
#12541=DIRECTION('',(-0.707106781186547,0.707106781186549,0.));
#12542=DIRECTION('center_axis',(0.,0.,1.));
#12543=DIRECTION('ref_axis',(1.,0.,0.));
#12544=DIRECTION('',(-0.707106781186547,-0.707106781186547,0.));
#12545=DIRECTION('center_axis',(0.,0.,1.));
#12546=DIRECTION('ref_axis',(1.,0.,0.));
#12547=DIRECTION('',(-0.707106781186547,-0.707106781186547,0.));
#12548=DIRECTION('center_axis',(0.707106781186548,-0.707106781186548,0.));
#12549=DIRECTION('ref_axis',(0.707106781186548,0.707106781186548,0.));
#12550=DIRECTION('center_axis',(1.,-1.80700362080917E-16,0.));
#12551=DIRECTION('ref_axis',(1.80700362080917E-16,1.,0.));
#12552=DIRECTION('',(-1.80700362080917E-16,-1.,0.));
#12553=DIRECTION('',(0.,0.,-1.));
#12554=DIRECTION('',(-1.80700362080917E-16,-1.,0.));
#12555=DIRECTION('center_axis',(-1.,1.80700362080917E-16,0.));
#12556=DIRECTION('ref_axis',(-1.80700362080917E-16,-1.,0.));
#12557=DIRECTION('',(1.80700362080917E-16,1.,0.));
#12558=DIRECTION('',(0.,0.,-1.));
#12559=DIRECTION('',(1.80700362080917E-16,1.,0.));
#12560=DIRECTION('center_axis',(0.,0.,1.));
#12561=DIRECTION('ref_axis',(1.,0.,0.));
#12562=DIRECTION('',(-1.,0.,0.));
#12563=DIRECTION('center_axis',(0.,0.,1.));
#12564=DIRECTION('ref_axis',(1.,0.,0.));
#12565=DIRECTION('',(-1.,0.,0.));
#12566=DIRECTION('center_axis',(0.,-1.,0.));
#12567=DIRECTION('ref_axis',(0.,0.,-1.));
#12568=DIRECTION('center_axis',(0.707106781186548,-0.707106781186547,0.));
#12569=DIRECTION('ref_axis',(0.707106781186547,0.707106781186548,0.));
#12570=DIRECTION('',(-0.707106781186547,-0.707106781186549,0.));
#12571=DIRECTION('',(0.,0.,-1.));
#12572=DIRECTION('',(-0.707106781186547,-0.707106781186549,0.));
#12573=DIRECTION('center_axis',(-0.707106781186547,0.707106781186548,0.));
#12574=DIRECTION('ref_axis',(-0.707106781186548,-0.707106781186547,0.));
#12575=DIRECTION('',(0.707106781186548,0.707106781186546,0.));
#12576=DIRECTION('',(0.,0.,-1.));
#12577=DIRECTION('',(0.707106781186548,0.707106781186546,0.));
#12578=DIRECTION('center_axis',(0.,0.,1.));
#12579=DIRECTION('ref_axis',(1.,0.,0.));
#12580=DIRECTION('',(-0.707106781186547,0.707106781186547,0.));
#12581=DIRECTION('center_axis',(0.,0.,1.));
#12582=DIRECTION('ref_axis',(1.,0.,0.));
#12583=DIRECTION('',(-0.707106781186547,0.707106781186547,0.));
#12584=DIRECTION('center_axis',(-0.707106781186548,-0.707106781186548,0.));
#12585=DIRECTION('ref_axis',(0.707106781186548,-0.707106781186548,0.));
#12586=DIRECTION('center_axis',(-1.35525271560688E-16,-1.,0.));
#12587=DIRECTION('ref_axis',(1.,-1.35525271560688E-16,0.));
#12588=DIRECTION('',(-1.,1.35525271560688E-16,0.));
#12589=DIRECTION('',(0.,0.,-1.));
#12590=DIRECTION('',(-1.,1.35525271560688E-16,0.));
#12591=DIRECTION('center_axis',(1.20466908053945E-16,1.,0.));
#12592=DIRECTION('ref_axis',(-1.,1.20466908053945E-16,0.));
#12593=DIRECTION('',(1.,-1.20466908053945E-16,0.));
#12594=DIRECTION('',(0.,0.,-1.));
#12595=DIRECTION('',(1.,-1.20466908053945E-16,0.));
#12596=DIRECTION('center_axis',(0.,0.,1.));
#12597=DIRECTION('ref_axis',(1.,0.,0.));
#12598=DIRECTION('',(0.,1.,0.));
#12599=DIRECTION('center_axis',(0.,0.,1.));
#12600=DIRECTION('ref_axis',(1.,0.,0.));
#12601=DIRECTION('',(0.,1.,0.));
#12602=DIRECTION('center_axis',(-1.,0.,0.));
#12603=DIRECTION('ref_axis',(0.,0.,1.));
#12604=DIRECTION('center_axis',(-0.707106781186547,-0.707106781186548,0.));
#12605=DIRECTION('ref_axis',(0.707106781186548,-0.707106781186547,0.));
#12606=DIRECTION('',(-0.707106781186548,0.707106781186546,0.));
#12607=DIRECTION('',(0.,0.,-1.));
#12608=DIRECTION('',(-0.707106781186548,0.707106781186546,0.));
#12609=DIRECTION('center_axis',(0.707106781186548,0.707106781186547,0.));
#12610=DIRECTION('ref_axis',(-0.707106781186547,0.707106781186548,0.));
#12611=DIRECTION('',(0.707106781186547,-0.707106781186549,0.));
#12612=DIRECTION('',(0.,0.,-1.));
#12613=DIRECTION('',(0.707106781186547,-0.707106781186549,0.));
#12614=DIRECTION('center_axis',(0.,0.,1.));
#12615=DIRECTION('ref_axis',(1.,0.,0.));
#12616=DIRECTION('',(0.707106781186547,0.707106781186547,0.));
#12617=DIRECTION('center_axis',(0.,0.,1.));
#12618=DIRECTION('ref_axis',(1.,0.,0.));
#12619=DIRECTION('',(0.707106781186547,0.707106781186547,0.));
#12620=DIRECTION('center_axis',(-0.707106781186548,0.707106781186548,0.));
#12621=DIRECTION('ref_axis',(-0.707106781186548,-0.707106781186548,0.));
#12622=DIRECTION('center_axis',(-1.,6.02334540269724E-17,0.));
#12623=DIRECTION('ref_axis',(-6.02334540269724E-17,-1.,0.));
#12624=DIRECTION('',(6.02334540269724E-17,1.,0.));
#12625=DIRECTION('',(0.,0.,-1.));
#12626=DIRECTION('',(6.02334540269724E-17,1.,0.));
#12627=DIRECTION('center_axis',(1.,-6.02334540269724E-17,0.));
#12628=DIRECTION('ref_axis',(6.02334540269724E-17,1.,0.));
#12629=DIRECTION('',(-6.02334540269724E-17,-1.,0.));
#12630=DIRECTION('',(0.,0.,-1.));
#12631=DIRECTION('',(-6.02334540269724E-17,-1.,0.));
#12632=DIRECTION('center_axis',(0.,0.,1.));
#12633=DIRECTION('ref_axis',(1.,0.,0.));
#12634=DIRECTION('',(1.,0.,0.));
#12635=DIRECTION('center_axis',(0.,0.,1.));
#12636=DIRECTION('ref_axis',(1.,0.,0.));
#12637=DIRECTION('',(1.,0.,0.));
#12638=DIRECTION('center_axis',(0.,1.,0.));
#12639=DIRECTION('ref_axis',(0.,0.,1.));
#12640=DIRECTION('center_axis',(-0.707106781186548,0.707106781186547,0.));
#12641=DIRECTION('ref_axis',(-0.707106781186547,-0.707106781186548,0.));
#12642=DIRECTION('',(0.707106781186547,0.707106781186549,0.));
#12643=DIRECTION('',(0.,0.,-1.));
#12644=DIRECTION('',(0.707106781186547,0.707106781186549,0.));
#12645=DIRECTION('center_axis',(0.707106781186547,-0.707106781186548,0.));
#12646=DIRECTION('ref_axis',(0.707106781186548,0.707106781186547,0.));
#12647=DIRECTION('',(-0.707106781186548,-0.707106781186546,0.));
#12648=DIRECTION('',(0.,0.,-1.));
#12649=DIRECTION('',(-0.707106781186548,-0.707106781186546,0.));
#12650=DIRECTION('center_axis',(0.,0.,1.));
#12651=DIRECTION('ref_axis',(1.,0.,0.));
#12652=DIRECTION('',(0.707106781186547,-0.707106781186547,0.));
#12653=DIRECTION('center_axis',(0.,0.,1.));
#12654=DIRECTION('ref_axis',(1.,0.,0.));
#12655=DIRECTION('',(0.707106781186547,-0.707106781186547,0.));
#12656=DIRECTION('center_axis',(0.707106781186548,0.707106781186548,0.));
#12657=DIRECTION('ref_axis',(-0.707106781186548,0.707106781186548,0.));
#12658=DIRECTION('center_axis',(0.,1.,0.));
#12659=DIRECTION('ref_axis',(0.,0.,1.));
#12660=DIRECTION('',(1.,0.,0.));
#12661=DIRECTION('',(0.,0.,-1.));
#12662=DIRECTION('',(1.,0.,0.));
#12663=DIRECTION('center_axis',(0.,-1.,0.));
#12664=DIRECTION('ref_axis',(0.,0.,-1.));
#12665=DIRECTION('',(-1.,0.,0.));
#12666=DIRECTION('',(0.,0.,-1.));
#12667=DIRECTION('',(-1.,0.,0.));
#12668=DIRECTION('center_axis',(0.,0.,1.));
#12669=DIRECTION('ref_axis',(1.,0.,0.));
#12670=DIRECTION('',(0.,-1.,0.));
#12671=DIRECTION('center_axis',(0.,0.,1.));
#12672=DIRECTION('ref_axis',(1.,0.,0.));
#12673=DIRECTION('',(0.,-1.,0.));
#12674=DIRECTION('center_axis',(1.,0.,0.));
#12675=DIRECTION('ref_axis',(0.,0.,-1.));
#12676=DIRECTION('center_axis',(-0.156434465040231,0.987688340595138,0.));
#12677=DIRECTION('ref_axis',(-0.987688340595138,-0.156434465040231,0.));
#12678=DIRECTION('',(0.987688340595138,0.156434465040231,0.));
#12679=DIRECTION('',(0.,0.,-1.));
#12680=DIRECTION('',(0.987688340595138,0.156434465040231,0.));
#12681=DIRECTION('center_axis',(0.156434465040231,-0.987688340595138,0.));
#12682=DIRECTION('ref_axis',(0.987688340595138,0.156434465040231,0.));
#12683=DIRECTION('',(-0.987688340595138,-0.156434465040231,0.));
#12684=DIRECTION('',(0.,0.,-1.));
#12685=DIRECTION('',(-0.987688340595138,-0.156434465040231,0.));
#12686=DIRECTION('center_axis',(0.,0.,1.));
#12687=DIRECTION('ref_axis',(1.,0.,0.));
#12688=DIRECTION('',(0.156434465040223,-0.987688340595139,0.));
#12689=DIRECTION('center_axis',(0.,0.,1.));
#12690=DIRECTION('ref_axis',(1.,0.,0.));
#12691=DIRECTION('',(0.156434465040223,-0.987688340595139,0.));
#12692=DIRECTION('center_axis',(0.987688340595139,0.156434465040223,0.));
#12693=DIRECTION('ref_axis',(-0.156434465040223,0.987688340595139,0.));
#12694=DIRECTION('center_axis',(0.156434465040232,0.987688340595138,0.));
#12695=DIRECTION('ref_axis',(-0.987688340595138,0.156434465040232,0.));
#12696=DIRECTION('',(0.987688340595138,-0.156434465040232,0.));
#12697=DIRECTION('',(0.,0.,-1.));
#12698=DIRECTION('',(0.987688340595138,-0.156434465040232,0.));
#12699=DIRECTION('center_axis',(-0.156434465040231,-0.987688340595138,0.));
#12700=DIRECTION('ref_axis',(0.987688340595138,-0.156434465040231,0.));
#12701=DIRECTION('',(-0.987688340595138,0.156434465040231,0.));
#12702=DIRECTION('',(0.,0.,-1.));
#12703=DIRECTION('',(-0.987688340595138,0.156434465040231,0.));
#12704=DIRECTION('center_axis',(0.,0.,1.));
#12705=DIRECTION('ref_axis',(1.,0.,0.));
#12706=DIRECTION('',(-0.156434465040224,-0.987688340595139,0.));
#12707=DIRECTION('center_axis',(0.,0.,1.));
#12708=DIRECTION('ref_axis',(1.,0.,0.));
#12709=DIRECTION('',(-0.156434465040224,-0.987688340595139,0.));
#12710=DIRECTION('center_axis',(0.987688340595139,-0.156434465040224,0.));
#12711=DIRECTION('ref_axis',(0.156434465040224,0.987688340595139,0.));
#12712=DIRECTION('center_axis',(0.309016994374948,0.951056516295154,0.));
#12713=DIRECTION('ref_axis',(-0.951056516295154,0.309016994374948,0.));
#12714=DIRECTION('',(0.951056516295153,-0.309016994374948,0.));
#12715=DIRECTION('',(0.,0.,-1.));
#12716=DIRECTION('',(0.951056516295153,-0.309016994374948,0.));
#12717=DIRECTION('center_axis',(-0.309016994374947,-0.951056516295154,0.));
#12718=DIRECTION('ref_axis',(0.951056516295154,-0.309016994374947,0.));
#12719=DIRECTION('',(-0.951056516295154,0.309016994374947,0.));
#12720=DIRECTION('',(0.,0.,-1.));
#12721=DIRECTION('',(-0.951056516295154,0.309016994374947,0.));
#12722=DIRECTION('center_axis',(0.,0.,1.));
#12723=DIRECTION('ref_axis',(1.,0.,0.));
#12724=DIRECTION('',(-0.309016994374941,-0.951056516295156,0.));
#12725=DIRECTION('center_axis',(0.,0.,1.));
#12726=DIRECTION('ref_axis',(1.,0.,0.));
#12727=DIRECTION('',(-0.309016994374941,-0.951056516295156,0.));
#12728=DIRECTION('center_axis',(0.951056516295156,-0.309016994374941,0.));
#12729=DIRECTION('ref_axis',(0.309016994374941,0.951056516295156,0.));
#12730=DIRECTION('center_axis',(0.453990499739548,0.891006524188367,0.));
#12731=DIRECTION('ref_axis',(-0.891006524188367,0.453990499739548,0.));
#12732=DIRECTION('',(0.891006524188367,-0.453990499739548,0.));
#12733=DIRECTION('',(0.,0.,-1.));
#12734=DIRECTION('',(0.891006524188367,-0.453990499739548,0.));
#12735=DIRECTION('center_axis',(-0.453990499739548,-0.891006524188367,0.));
#12736=DIRECTION('ref_axis',(0.891006524188367,-0.453990499739548,0.));
#12737=DIRECTION('',(-0.891006524188367,0.453990499739548,0.));
#12738=DIRECTION('',(0.,0.,-1.));
#12739=DIRECTION('',(-0.891006524188367,0.453990499739548,0.));
#12740=DIRECTION('center_axis',(0.,0.,1.));
#12741=DIRECTION('ref_axis',(1.,0.,0.));
#12742=DIRECTION('',(-0.453990499739554,-0.891006524188364,0.));
#12743=DIRECTION('center_axis',(0.,0.,1.));
#12744=DIRECTION('ref_axis',(1.,0.,0.));
#12745=DIRECTION('',(-0.453990499739554,-0.891006524188364,0.));
#12746=DIRECTION('center_axis',(0.891006524188364,-0.453990499739554,0.));
#12747=DIRECTION('ref_axis',(0.453990499739554,0.891006524188364,0.));
#12748=DIRECTION('center_axis',(0.587785252292473,0.809016994374947,0.));
#12749=DIRECTION('ref_axis',(-0.809016994374947,0.587785252292473,0.));
#12750=DIRECTION('',(0.809016994374947,-0.587785252292473,0.));
#12751=DIRECTION('',(0.,0.,-1.));
#12752=DIRECTION('',(0.809016994374947,-0.587785252292473,0.));
#12753=DIRECTION('center_axis',(-0.587785252292474,-0.809016994374946,0.));
#12754=DIRECTION('ref_axis',(0.809016994374946,-0.587785252292474,0.));
#12755=DIRECTION('',(-0.809016994374946,0.587785252292474,0.));
#12756=DIRECTION('',(0.,0.,-1.));
#12757=DIRECTION('',(-0.809016994374946,0.587785252292474,0.));
#12758=DIRECTION('center_axis',(0.,0.,1.));
#12759=DIRECTION('ref_axis',(1.,0.,0.));
#12760=DIRECTION('',(-0.587785252292475,-0.809016994374946,0.));
#12761=DIRECTION('center_axis',(0.,0.,1.));
#12762=DIRECTION('ref_axis',(1.,0.,0.));
#12763=DIRECTION('',(-0.587785252292475,-0.809016994374946,0.));
#12764=DIRECTION('center_axis',(0.809016994374946,-0.587785252292475,0.));
#12765=DIRECTION('ref_axis',(0.587785252292475,0.809016994374946,0.));
#12766=DIRECTION('center_axis',(0.809016994374948,0.587785252292472,0.));
#12767=DIRECTION('ref_axis',(-0.587785252292472,0.809016994374948,0.));
#12768=DIRECTION('',(0.587785252292472,-0.809016994374948,0.));
#12769=DIRECTION('',(0.,0.,-1.));
#12770=DIRECTION('',(0.587785252292472,-0.809016994374948,0.));
#12771=DIRECTION('center_axis',(-0.809016994374948,-0.587785252292472,0.));
#12772=DIRECTION('ref_axis',(0.587785252292472,-0.809016994374948,0.));
#12773=DIRECTION('',(-0.587785252292472,0.809016994374948,0.));
#12774=DIRECTION('',(0.,0.,-1.));
#12775=DIRECTION('',(-0.587785252292472,0.809016994374948,0.));
#12776=DIRECTION('center_axis',(0.,0.,1.));
#12777=DIRECTION('ref_axis',(1.,0.,0.));
#12778=DIRECTION('',(-0.809016994374946,-0.587785252292475,0.));
#12779=DIRECTION('center_axis',(0.,0.,1.));
#12780=DIRECTION('ref_axis',(1.,0.,0.));
#12781=DIRECTION('',(-0.809016994374946,-0.587785252292475,0.));
#12782=DIRECTION('center_axis',(0.587785252292475,-0.809016994374946,0.));
#12783=DIRECTION('ref_axis',(0.809016994374946,0.587785252292475,0.));
#12784=DIRECTION('center_axis',(0.891006524188367,0.453990499739548,0.));
#12785=DIRECTION('ref_axis',(-0.453990499739548,0.891006524188367,0.));
#12786=DIRECTION('',(0.453990499739548,-0.891006524188367,0.));
#12787=DIRECTION('',(0.,0.,-1.));
#12788=DIRECTION('',(0.453990499739548,-0.891006524188367,0.));
#12789=DIRECTION('center_axis',(-0.891006524188367,-0.453990499739548,0.));
#12790=DIRECTION('ref_axis',(0.453990499739548,-0.891006524188367,0.));
#12791=DIRECTION('',(-0.453990499739548,0.891006524188367,0.));
#12792=DIRECTION('',(0.,0.,-1.));
#12793=DIRECTION('',(-0.453990499739548,0.891006524188367,0.));
#12794=DIRECTION('center_axis',(0.,0.,1.));
#12795=DIRECTION('ref_axis',(1.,0.,0.));
#12796=DIRECTION('',(-0.891006524188364,-0.453990499739554,0.));
#12797=DIRECTION('center_axis',(0.,0.,1.));
#12798=DIRECTION('ref_axis',(1.,0.,0.));
#12799=DIRECTION('',(-0.891006524188364,-0.453990499739554,0.));
#12800=DIRECTION('center_axis',(0.453990499739554,-0.891006524188364,0.));
#12801=DIRECTION('ref_axis',(0.891006524188364,0.453990499739554,0.));
#12802=DIRECTION('center_axis',(0.951056516295154,0.309016994374947,0.));
#12803=DIRECTION('ref_axis',(-0.309016994374947,0.951056516295154,0.));
#12804=DIRECTION('',(0.309016994374947,-0.951056516295154,0.));
#12805=DIRECTION('',(0.,0.,-1.));
#12806=DIRECTION('',(0.309016994374947,-0.951056516295154,0.));
#12807=DIRECTION('center_axis',(-0.951056516295154,-0.309016994374947,0.));
#12808=DIRECTION('ref_axis',(0.309016994374947,-0.951056516295154,0.));
#12809=DIRECTION('',(-0.309016994374947,0.951056516295154,0.));
#12810=DIRECTION('',(0.,0.,-1.));
#12811=DIRECTION('',(-0.309016994374947,0.951056516295154,0.));
#12812=DIRECTION('center_axis',(0.,0.,1.));
#12813=DIRECTION('ref_axis',(1.,0.,0.));
#12814=DIRECTION('',(-0.951056516295156,-0.309016994374941,0.));
#12815=DIRECTION('center_axis',(0.,0.,1.));
#12816=DIRECTION('ref_axis',(1.,0.,0.));
#12817=DIRECTION('',(-0.951056516295156,-0.309016994374941,0.));
#12818=DIRECTION('center_axis',(0.309016994374941,-0.951056516295156,0.));
#12819=DIRECTION('ref_axis',(0.951056516295156,0.309016994374941,0.));
#12820=DIRECTION('center_axis',(0.987688340595138,0.156434465040231,0.));
#12821=DIRECTION('ref_axis',(-0.156434465040231,0.987688340595138,0.));
#12822=DIRECTION('',(0.156434465040231,-0.987688340595138,0.));
#12823=DIRECTION('',(0.,0.,-1.));
#12824=DIRECTION('',(0.156434465040231,-0.987688340595138,0.));
#12825=DIRECTION('center_axis',(-0.987688340595138,-0.156434465040231,0.));
#12826=DIRECTION('ref_axis',(0.156434465040231,-0.987688340595138,0.));
#12827=DIRECTION('',(-0.156434465040231,0.987688340595138,0.));
#12828=DIRECTION('',(0.,0.,-1.));
#12829=DIRECTION('',(-0.156434465040231,0.987688340595138,0.));
#12830=DIRECTION('center_axis',(0.,0.,1.));
#12831=DIRECTION('ref_axis',(1.,0.,0.));
#12832=DIRECTION('',(-0.987688340595139,-0.156434465040223,0.));
#12833=DIRECTION('center_axis',(0.,0.,1.));
#12834=DIRECTION('ref_axis',(1.,0.,0.));
#12835=DIRECTION('',(-0.987688340595139,-0.156434465040223,0.));
#12836=DIRECTION('center_axis',(0.156434465040223,-0.987688340595139,0.));
#12837=DIRECTION('ref_axis',(0.987688340595139,0.156434465040223,0.));
#12838=DIRECTION('center_axis',(0.987688340595138,-0.156434465040231,0.));
#12839=DIRECTION('ref_axis',(0.156434465040231,0.987688340595138,0.));
#12840=DIRECTION('',(-0.156434465040231,-0.987688340595138,0.));
#12841=DIRECTION('',(0.,0.,-1.));
#12842=DIRECTION('',(-0.156434465040231,-0.987688340595138,0.));
#12843=DIRECTION('center_axis',(-0.987688340595138,0.156434465040231,0.));
#12844=DIRECTION('ref_axis',(-0.156434465040231,-0.987688340595138,0.));
#12845=DIRECTION('',(0.156434465040231,0.987688340595138,0.));
#12846=DIRECTION('',(0.,0.,-1.));
#12847=DIRECTION('',(0.156434465040231,0.987688340595138,0.));
#12848=DIRECTION('center_axis',(0.,0.,1.));
#12849=DIRECTION('ref_axis',(1.,0.,0.));
#12850=DIRECTION('',(-0.987688340595139,0.156434465040224,0.));
#12851=DIRECTION('center_axis',(0.,0.,1.));
#12852=DIRECTION('ref_axis',(1.,0.,0.));
#12853=DIRECTION('',(-0.987688340595139,0.156434465040224,0.));
#12854=DIRECTION('center_axis',(-0.156434465040224,-0.987688340595139,0.));
#12855=DIRECTION('ref_axis',(0.987688340595139,-0.156434465040224,0.));
#12856=DIRECTION('center_axis',(0.951056516295154,-0.309016994374948,0.));
#12857=DIRECTION('ref_axis',(0.309016994374948,0.951056516295154,0.));
#12858=DIRECTION('',(-0.309016994374948,-0.951056516295153,0.));
#12859=DIRECTION('',(0.,0.,-1.));
#12860=DIRECTION('',(-0.309016994374948,-0.951056516295153,0.));
#12861=DIRECTION('center_axis',(-0.951056516295154,0.309016994374947,0.));
#12862=DIRECTION('ref_axis',(-0.309016994374947,-0.951056516295154,0.));
#12863=DIRECTION('',(0.309016994374947,0.951056516295154,0.));
#12864=DIRECTION('',(0.,0.,-1.));
#12865=DIRECTION('',(0.309016994374947,0.951056516295154,0.));
#12866=DIRECTION('center_axis',(0.,0.,1.));
#12867=DIRECTION('ref_axis',(1.,0.,0.));
#12868=DIRECTION('',(-0.951056516295156,0.309016994374941,0.));
#12869=DIRECTION('center_axis',(0.,0.,1.));
#12870=DIRECTION('ref_axis',(1.,0.,0.));
#12871=DIRECTION('',(-0.951056516295156,0.309016994374941,0.));
#12872=DIRECTION('center_axis',(-0.309016994374941,-0.951056516295156,0.));
#12873=DIRECTION('ref_axis',(0.951056516295156,-0.309016994374941,0.));
#12874=DIRECTION('center_axis',(0.891006524188367,-0.453990499739548,0.));
#12875=DIRECTION('ref_axis',(0.453990499739548,0.891006524188367,0.));
#12876=DIRECTION('',(-0.453990499739548,-0.891006524188367,0.));
#12877=DIRECTION('',(0.,0.,-1.));
#12878=DIRECTION('',(-0.453990499739548,-0.891006524188367,0.));
#12879=DIRECTION('center_axis',(-0.891006524188367,0.453990499739548,0.));
#12880=DIRECTION('ref_axis',(-0.453990499739548,-0.891006524188367,0.));
#12881=DIRECTION('',(0.453990499739548,0.891006524188367,0.));
#12882=DIRECTION('',(0.,0.,-1.));
#12883=DIRECTION('',(0.453990499739548,0.891006524188367,0.));
#12884=DIRECTION('center_axis',(0.,0.,1.));
#12885=DIRECTION('ref_axis',(1.,0.,0.));
#12886=DIRECTION('',(-0.891006524188364,0.453990499739554,0.));
#12887=DIRECTION('center_axis',(0.,0.,1.));
#12888=DIRECTION('ref_axis',(1.,0.,0.));
#12889=DIRECTION('',(-0.891006524188364,0.453990499739554,0.));
#12890=DIRECTION('center_axis',(-0.453990499739554,-0.891006524188364,0.));
#12891=DIRECTION('ref_axis',(0.891006524188364,-0.453990499739554,0.));
#12892=DIRECTION('center_axis',(0.809016994374947,-0.587785252292473,0.));
#12893=DIRECTION('ref_axis',(0.587785252292473,0.809016994374947,0.));
#12894=DIRECTION('',(-0.587785252292473,-0.809016994374947,0.));
#12895=DIRECTION('',(0.,0.,-1.));
#12896=DIRECTION('',(-0.587785252292473,-0.809016994374947,0.));
#12897=DIRECTION('center_axis',(-0.809016994374946,0.587785252292474,0.));
#12898=DIRECTION('ref_axis',(-0.587785252292474,-0.809016994374946,0.));
#12899=DIRECTION('',(0.587785252292474,0.809016994374946,0.));
#12900=DIRECTION('',(0.,0.,-1.));
#12901=DIRECTION('',(0.587785252292474,0.809016994374946,0.));
#12902=DIRECTION('center_axis',(0.,0.,1.));
#12903=DIRECTION('ref_axis',(1.,0.,0.));
#12904=DIRECTION('',(-0.809016994374946,0.587785252292475,0.));
#12905=DIRECTION('center_axis',(0.,0.,1.));
#12906=DIRECTION('ref_axis',(1.,0.,0.));
#12907=DIRECTION('',(-0.809016994374946,0.587785252292475,0.));
#12908=DIRECTION('center_axis',(-0.587785252292475,-0.809016994374946,0.));
#12909=DIRECTION('ref_axis',(0.809016994374946,-0.587785252292475,0.));
#12910=DIRECTION('center_axis',(0.587785252292472,-0.809016994374948,0.));
#12911=DIRECTION('ref_axis',(0.809016994374948,0.587785252292472,0.));
#12912=DIRECTION('',(-0.809016994374948,-0.587785252292472,0.));
#12913=DIRECTION('',(0.,0.,-1.));
#12914=DIRECTION('',(-0.809016994374948,-0.587785252292472,0.));
#12915=DIRECTION('center_axis',(-0.587785252292472,0.809016994374948,0.));
#12916=DIRECTION('ref_axis',(-0.809016994374948,-0.587785252292472,0.));
#12917=DIRECTION('',(0.809016994374948,0.587785252292472,0.));
#12918=DIRECTION('',(0.,0.,-1.));
#12919=DIRECTION('',(0.809016994374948,0.587785252292472,0.));
#12920=DIRECTION('center_axis',(0.,0.,1.));
#12921=DIRECTION('ref_axis',(1.,0.,0.));
#12922=DIRECTION('',(-0.587785252292475,0.809016994374946,0.));
#12923=DIRECTION('center_axis',(0.,0.,1.));
#12924=DIRECTION('ref_axis',(1.,0.,0.));
#12925=DIRECTION('',(-0.587785252292475,0.809016994374946,0.));
#12926=DIRECTION('center_axis',(-0.809016994374946,-0.587785252292475,0.));
#12927=DIRECTION('ref_axis',(0.587785252292475,-0.809016994374946,0.));
#12928=DIRECTION('center_axis',(0.453990499739548,-0.891006524188367,0.));
#12929=DIRECTION('ref_axis',(0.891006524188367,0.453990499739548,0.));
#12930=DIRECTION('',(-0.891006524188367,-0.453990499739548,0.));
#12931=DIRECTION('',(0.,0.,-1.));
#12932=DIRECTION('',(-0.891006524188367,-0.453990499739548,0.));
#12933=DIRECTION('center_axis',(-0.453990499739548,0.891006524188367,0.));
#12934=DIRECTION('ref_axis',(-0.891006524188367,-0.453990499739548,0.));
#12935=DIRECTION('',(0.891006524188367,0.453990499739548,0.));
#12936=DIRECTION('',(0.,0.,-1.));
#12937=DIRECTION('',(0.891006524188367,0.453990499739548,0.));
#12938=DIRECTION('center_axis',(0.,0.,1.));
#12939=DIRECTION('ref_axis',(1.,0.,0.));
#12940=DIRECTION('',(-0.453990499739554,0.891006524188364,0.));
#12941=DIRECTION('center_axis',(0.,0.,1.));
#12942=DIRECTION('ref_axis',(1.,0.,0.));
#12943=DIRECTION('',(-0.453990499739554,0.891006524188364,0.));
#12944=DIRECTION('center_axis',(-0.891006524188364,-0.453990499739554,0.));
#12945=DIRECTION('ref_axis',(0.453990499739554,-0.891006524188364,0.));
#12946=DIRECTION('center_axis',(0.309016994374947,-0.951056516295154,0.));
#12947=DIRECTION('ref_axis',(0.951056516295154,0.309016994374947,0.));
#12948=DIRECTION('',(-0.951056516295154,-0.309016994374947,0.));
#12949=DIRECTION('',(0.,0.,-1.));
#12950=DIRECTION('',(-0.951056516295154,-0.309016994374947,0.));
#12951=DIRECTION('center_axis',(-0.309016994374947,0.951056516295154,0.));
#12952=DIRECTION('ref_axis',(-0.951056516295154,-0.309016994374947,0.));
#12953=DIRECTION('',(0.951056516295154,0.309016994374947,0.));
#12954=DIRECTION('',(0.,0.,-1.));
#12955=DIRECTION('',(0.951056516295154,0.309016994374947,0.));
#12956=DIRECTION('center_axis',(0.,0.,1.));
#12957=DIRECTION('ref_axis',(1.,0.,0.));
#12958=DIRECTION('',(-0.309016994374941,0.951056516295156,0.));
#12959=DIRECTION('center_axis',(0.,0.,1.));
#12960=DIRECTION('ref_axis',(1.,0.,0.));
#12961=DIRECTION('',(-0.309016994374941,0.951056516295156,0.));
#12962=DIRECTION('center_axis',(-0.951056516295156,-0.309016994374941,0.));
#12963=DIRECTION('ref_axis',(0.309016994374941,-0.951056516295156,0.));
#12964=DIRECTION('center_axis',(0.156434465040231,-0.987688340595138,0.));
#12965=DIRECTION('ref_axis',(0.987688340595138,0.156434465040231,0.));
#12966=DIRECTION('',(-0.987688340595138,-0.156434465040231,0.));
#12967=DIRECTION('',(0.,0.,-1.));
#12968=DIRECTION('',(-0.987688340595138,-0.156434465040231,0.));
#12969=DIRECTION('center_axis',(-0.156434465040231,0.987688340595138,0.));
#12970=DIRECTION('ref_axis',(-0.987688340595138,-0.156434465040231,0.));
#12971=DIRECTION('',(0.987688340595138,0.156434465040231,0.));
#12972=DIRECTION('',(0.,0.,-1.));
#12973=DIRECTION('',(0.987688340595138,0.156434465040231,0.));
#12974=DIRECTION('center_axis',(0.,0.,1.));
#12975=DIRECTION('ref_axis',(1.,0.,0.));
#12976=DIRECTION('',(-0.156434465040223,0.987688340595139,0.));
#12977=DIRECTION('center_axis',(0.,0.,1.));
#12978=DIRECTION('ref_axis',(1.,0.,0.));
#12979=DIRECTION('',(-0.156434465040223,0.987688340595139,0.));
#12980=DIRECTION('center_axis',(-0.987688340595139,-0.156434465040223,0.));
#12981=DIRECTION('ref_axis',(0.156434465040223,-0.987688340595139,0.));
#12982=DIRECTION('center_axis',(-0.156434465040231,-0.987688340595138,0.));
#12983=DIRECTION('ref_axis',(0.987688340595138,-0.156434465040231,0.));
#12984=DIRECTION('',(-0.987688340595138,0.156434465040231,0.));
#12985=DIRECTION('',(0.,0.,-1.));
#12986=DIRECTION('',(-0.987688340595138,0.156434465040231,0.));
#12987=DIRECTION('center_axis',(0.156434465040231,0.987688340595138,0.));
#12988=DIRECTION('ref_axis',(-0.987688340595138,0.156434465040231,0.));
#12989=DIRECTION('',(0.987688340595138,-0.156434465040231,0.));
#12990=DIRECTION('',(0.,0.,-1.));
#12991=DIRECTION('',(0.987688340595138,-0.156434465040231,0.));
#12992=DIRECTION('center_axis',(0.,0.,1.));
#12993=DIRECTION('ref_axis',(1.,0.,0.));
#12994=DIRECTION('',(0.156434465040224,0.987688340595139,0.));
#12995=DIRECTION('center_axis',(0.,0.,1.));
#12996=DIRECTION('ref_axis',(1.,0.,0.));
#12997=DIRECTION('',(0.156434465040224,0.987688340595139,0.));
#12998=DIRECTION('center_axis',(-0.987688340595139,0.156434465040224,0.));
#12999=DIRECTION('ref_axis',(-0.156434465040224,-0.987688340595139,0.));
#13000=DIRECTION('center_axis',(-0.309016994374948,-0.951056516295154,0.));
#13001=DIRECTION('ref_axis',(0.951056516295154,-0.309016994374948,0.));
#13002=DIRECTION('',(-0.951056516295153,0.309016994374948,0.));
#13003=DIRECTION('',(0.,0.,-1.));
#13004=DIRECTION('',(-0.951056516295153,0.309016994374948,0.));
#13005=DIRECTION('center_axis',(0.309016994374947,0.951056516295154,0.));
#13006=DIRECTION('ref_axis',(-0.951056516295154,0.309016994374947,0.));
#13007=DIRECTION('',(0.951056516295154,-0.309016994374947,0.));
#13008=DIRECTION('',(0.,0.,-1.));
#13009=DIRECTION('',(0.951056516295154,-0.309016994374947,0.));
#13010=DIRECTION('center_axis',(0.,0.,1.));
#13011=DIRECTION('ref_axis',(1.,0.,0.));
#13012=DIRECTION('',(0.309016994374941,0.951056516295156,0.));
#13013=DIRECTION('center_axis',(0.,0.,1.));
#13014=DIRECTION('ref_axis',(1.,0.,0.));
#13015=DIRECTION('',(0.309016994374941,0.951056516295156,0.));
#13016=DIRECTION('center_axis',(-0.951056516295156,0.309016994374941,0.));
#13017=DIRECTION('ref_axis',(-0.309016994374941,-0.951056516295156,0.));
#13018=DIRECTION('center_axis',(-0.453990499739548,-0.891006524188367,0.));
#13019=DIRECTION('ref_axis',(0.891006524188367,-0.453990499739548,0.));
#13020=DIRECTION('',(-0.891006524188367,0.453990499739548,0.));
#13021=DIRECTION('',(0.,0.,-1.));
#13022=DIRECTION('',(-0.891006524188367,0.453990499739548,0.));
#13023=DIRECTION('center_axis',(0.453990499739548,0.891006524188367,0.));
#13024=DIRECTION('ref_axis',(-0.891006524188367,0.453990499739548,0.));
#13025=DIRECTION('',(0.891006524188367,-0.453990499739548,0.));
#13026=DIRECTION('',(0.,0.,-1.));
#13027=DIRECTION('',(0.891006524188367,-0.453990499739548,0.));
#13028=DIRECTION('center_axis',(0.,0.,1.));
#13029=DIRECTION('ref_axis',(1.,0.,0.));
#13030=DIRECTION('',(0.453990499739554,0.891006524188364,0.));
#13031=DIRECTION('center_axis',(0.,0.,1.));
#13032=DIRECTION('ref_axis',(1.,0.,0.));
#13033=DIRECTION('',(0.453990499739554,0.891006524188364,0.));
#13034=DIRECTION('center_axis',(-0.891006524188364,0.453990499739554,0.));
#13035=DIRECTION('ref_axis',(-0.453990499739554,-0.891006524188364,0.));
#13036=DIRECTION('center_axis',(-0.587785252292473,-0.809016994374947,0.));
#13037=DIRECTION('ref_axis',(0.809016994374947,-0.587785252292473,0.));
#13038=DIRECTION('',(-0.809016994374947,0.587785252292473,0.));
#13039=DIRECTION('',(0.,0.,-1.));
#13040=DIRECTION('',(-0.809016994374947,0.587785252292473,0.));
#13041=DIRECTION('center_axis',(0.587785252292474,0.809016994374946,0.));
#13042=DIRECTION('ref_axis',(-0.809016994374946,0.587785252292474,0.));
#13043=DIRECTION('',(0.809016994374946,-0.587785252292474,0.));
#13044=DIRECTION('',(0.,0.,-1.));
#13045=DIRECTION('',(0.809016994374946,-0.587785252292474,0.));
#13046=DIRECTION('center_axis',(0.,0.,1.));
#13047=DIRECTION('ref_axis',(1.,0.,0.));
#13048=DIRECTION('',(0.587785252292475,0.809016994374946,0.));
#13049=DIRECTION('center_axis',(0.,0.,1.));
#13050=DIRECTION('ref_axis',(1.,0.,0.));
#13051=DIRECTION('',(0.587785252292475,0.809016994374946,0.));
#13052=DIRECTION('center_axis',(-0.809016994374946,0.587785252292475,0.));
#13053=DIRECTION('ref_axis',(-0.587785252292475,-0.809016994374946,0.));
#13054=DIRECTION('center_axis',(-0.809016994374948,-0.587785252292472,0.));
#13055=DIRECTION('ref_axis',(0.587785252292472,-0.809016994374948,0.));
#13056=DIRECTION('',(-0.587785252292472,0.809016994374948,0.));
#13057=DIRECTION('',(0.,0.,-1.));
#13058=DIRECTION('',(-0.587785252292472,0.809016994374948,0.));
#13059=DIRECTION('center_axis',(0.809016994374948,0.587785252292472,0.));
#13060=DIRECTION('ref_axis',(-0.587785252292472,0.809016994374948,0.));
#13061=DIRECTION('',(0.587785252292472,-0.809016994374948,0.));
#13062=DIRECTION('',(0.,0.,-1.));
#13063=DIRECTION('',(0.587785252292472,-0.809016994374948,0.));
#13064=DIRECTION('center_axis',(0.,0.,1.));
#13065=DIRECTION('ref_axis',(1.,0.,0.));
#13066=DIRECTION('',(0.809016994374946,0.587785252292475,0.));
#13067=DIRECTION('center_axis',(0.,0.,1.));
#13068=DIRECTION('ref_axis',(1.,0.,0.));
#13069=DIRECTION('',(0.809016994374946,0.587785252292475,0.));
#13070=DIRECTION('center_axis',(-0.587785252292475,0.809016994374946,0.));
#13071=DIRECTION('ref_axis',(-0.809016994374946,-0.587785252292475,0.));
#13072=DIRECTION('center_axis',(-0.891006524188367,-0.453990499739548,0.));
#13073=DIRECTION('ref_axis',(0.453990499739548,-0.891006524188367,0.));
#13074=DIRECTION('',(-0.453990499739548,0.891006524188367,0.));
#13075=DIRECTION('',(0.,0.,-1.));
#13076=DIRECTION('',(-0.453990499739548,0.891006524188367,0.));
#13077=DIRECTION('center_axis',(0.891006524188367,0.453990499739548,0.));
#13078=DIRECTION('ref_axis',(-0.453990499739548,0.891006524188367,0.));
#13079=DIRECTION('',(0.453990499739548,-0.891006524188367,0.));
#13080=DIRECTION('',(0.,0.,-1.));
#13081=DIRECTION('',(0.453990499739548,-0.891006524188367,0.));
#13082=DIRECTION('center_axis',(0.,0.,1.));
#13083=DIRECTION('ref_axis',(1.,0.,0.));
#13084=DIRECTION('',(0.891006524188364,0.453990499739554,0.));
#13085=DIRECTION('center_axis',(0.,0.,1.));
#13086=DIRECTION('ref_axis',(1.,0.,0.));
#13087=DIRECTION('',(0.891006524188364,0.453990499739554,0.));
#13088=DIRECTION('center_axis',(-0.453990499739554,0.891006524188364,0.));
#13089=DIRECTION('ref_axis',(-0.891006524188364,-0.453990499739554,0.));
#13090=DIRECTION('center_axis',(-0.951056516295154,-0.309016994374947,0.));
#13091=DIRECTION('ref_axis',(0.309016994374947,-0.951056516295154,0.));
#13092=DIRECTION('',(-0.309016994374947,0.951056516295154,0.));
#13093=DIRECTION('',(0.,0.,-1.));
#13094=DIRECTION('',(-0.309016994374947,0.951056516295154,0.));
#13095=DIRECTION('center_axis',(0.951056516295154,0.309016994374947,0.));
#13096=DIRECTION('ref_axis',(-0.309016994374947,0.951056516295154,0.));
#13097=DIRECTION('',(0.309016994374947,-0.951056516295154,0.));
#13098=DIRECTION('',(0.,0.,-1.));
#13099=DIRECTION('',(0.309016994374947,-0.951056516295154,0.));
#13100=DIRECTION('center_axis',(0.,0.,1.));
#13101=DIRECTION('ref_axis',(1.,0.,0.));
#13102=DIRECTION('',(0.951056516295156,0.309016994374941,0.));
#13103=DIRECTION('center_axis',(0.,0.,1.));
#13104=DIRECTION('ref_axis',(1.,0.,0.));
#13105=DIRECTION('',(0.951056516295156,0.309016994374941,0.));
#13106=DIRECTION('center_axis',(-0.309016994374941,0.951056516295156,0.));
#13107=DIRECTION('ref_axis',(-0.951056516295156,-0.309016994374941,0.));
#13108=DIRECTION('center_axis',(-0.987688340595138,-0.156434465040231,0.));
#13109=DIRECTION('ref_axis',(0.156434465040231,-0.987688340595138,0.));
#13110=DIRECTION('',(-0.156434465040231,0.987688340595138,0.));
#13111=DIRECTION('',(0.,0.,-1.));
#13112=DIRECTION('',(-0.156434465040231,0.987688340595138,0.));
#13113=DIRECTION('center_axis',(0.987688340595138,0.156434465040231,0.));
#13114=DIRECTION('ref_axis',(-0.156434465040231,0.987688340595138,0.));
#13115=DIRECTION('',(0.156434465040231,-0.987688340595138,0.));
#13116=DIRECTION('',(0.,0.,-1.));
#13117=DIRECTION('',(0.156434465040231,-0.987688340595138,0.));
#13118=DIRECTION('center_axis',(0.,0.,1.));
#13119=DIRECTION('ref_axis',(1.,0.,0.));
#13120=DIRECTION('',(0.987688340595139,0.156434465040223,0.));
#13121=DIRECTION('center_axis',(0.,0.,1.));
#13122=DIRECTION('ref_axis',(1.,0.,0.));
#13123=DIRECTION('',(0.987688340595139,0.156434465040223,0.));
#13124=DIRECTION('center_axis',(-0.156434465040223,0.987688340595139,0.));
#13125=DIRECTION('ref_axis',(-0.987688340595139,-0.156434465040223,0.));
#13126=DIRECTION('center_axis',(-0.987688340595138,0.156434465040231,0.));
#13127=DIRECTION('ref_axis',(-0.156434465040231,-0.987688340595138,0.));
#13128=DIRECTION('',(0.156434465040231,0.987688340595138,0.));
#13129=DIRECTION('',(0.,0.,-1.));
#13130=DIRECTION('',(0.156434465040231,0.987688340595138,0.));
#13131=DIRECTION('center_axis',(0.987688340595138,-0.156434465040232,0.));
#13132=DIRECTION('ref_axis',(0.156434465040232,0.987688340595138,0.));
#13133=DIRECTION('',(-0.156434465040232,-0.987688340595138,0.));
#13134=DIRECTION('',(0.,0.,-1.));
#13135=DIRECTION('',(-0.156434465040232,-0.987688340595138,0.));
#13136=DIRECTION('center_axis',(0.,0.,1.));
#13137=DIRECTION('ref_axis',(1.,0.,0.));
#13138=DIRECTION('',(0.987688340595139,-0.156434465040223,0.));
#13139=DIRECTION('center_axis',(0.,0.,1.));
#13140=DIRECTION('ref_axis',(1.,0.,0.));
#13141=DIRECTION('',(0.987688340595139,-0.156434465040223,0.));
#13142=DIRECTION('center_axis',(0.156434465040223,0.987688340595139,0.));
#13143=DIRECTION('ref_axis',(-0.987688340595139,0.156434465040223,0.));
#13144=DIRECTION('center_axis',(-0.951056516295154,0.309016994374948,0.));
#13145=DIRECTION('ref_axis',(-0.309016994374948,-0.951056516295154,0.));
#13146=DIRECTION('',(0.309016994374948,0.951056516295153,0.));
#13147=DIRECTION('',(0.,0.,-1.));
#13148=DIRECTION('',(0.309016994374948,0.951056516295153,0.));
#13149=DIRECTION('center_axis',(0.951056516295154,-0.309016994374947,0.));
#13150=DIRECTION('ref_axis',(0.309016994374947,0.951056516295154,0.));
#13151=DIRECTION('',(-0.309016994374947,-0.951056516295154,0.));
#13152=DIRECTION('',(0.,0.,-1.));
#13153=DIRECTION('',(-0.309016994374947,-0.951056516295154,0.));
#13154=DIRECTION('center_axis',(0.,0.,1.));
#13155=DIRECTION('ref_axis',(1.,0.,0.));
#13156=DIRECTION('',(0.951056516295156,-0.309016994374941,0.));
#13157=DIRECTION('center_axis',(0.,0.,1.));
#13158=DIRECTION('ref_axis',(1.,0.,0.));
#13159=DIRECTION('',(0.951056516295156,-0.309016994374941,0.));
#13160=DIRECTION('center_axis',(0.309016994374941,0.951056516295156,0.));
#13161=DIRECTION('ref_axis',(-0.951056516295156,0.309016994374941,0.));
#13162=DIRECTION('center_axis',(-0.891006524188367,0.453990499739548,0.));
#13163=DIRECTION('ref_axis',(-0.453990499739548,-0.891006524188367,0.));
#13164=DIRECTION('',(0.453990499739548,0.891006524188367,0.));
#13165=DIRECTION('',(0.,0.,-1.));
#13166=DIRECTION('',(0.453990499739548,0.891006524188367,0.));
#13167=DIRECTION('center_axis',(0.891006524188367,-0.453990499739548,0.));
#13168=DIRECTION('ref_axis',(0.453990499739548,0.891006524188367,0.));
#13169=DIRECTION('',(-0.453990499739548,-0.891006524188367,0.));
#13170=DIRECTION('',(0.,0.,-1.));
#13171=DIRECTION('',(-0.453990499739548,-0.891006524188367,0.));
#13172=DIRECTION('center_axis',(0.,0.,1.));
#13173=DIRECTION('ref_axis',(1.,0.,0.));
#13174=DIRECTION('',(0.891006524188364,-0.453990499739554,0.));
#13175=DIRECTION('center_axis',(0.,0.,1.));
#13176=DIRECTION('ref_axis',(1.,0.,0.));
#13177=DIRECTION('',(0.891006524188364,-0.453990499739554,0.));
#13178=DIRECTION('center_axis',(0.453990499739554,0.891006524188364,0.));
#13179=DIRECTION('ref_axis',(-0.891006524188364,0.453990499739554,0.));
#13180=DIRECTION('center_axis',(-0.809016994374948,0.587785252292472,0.));
#13181=DIRECTION('ref_axis',(-0.587785252292472,-0.809016994374948,0.));
#13182=DIRECTION('',(0.587785252292472,0.809016994374948,0.));
#13183=DIRECTION('',(0.,0.,-1.));
#13184=DIRECTION('',(0.587785252292472,0.809016994374948,0.));
#13185=DIRECTION('center_axis',(0.809016994374948,-0.587785252292472,0.));
#13186=DIRECTION('ref_axis',(0.587785252292472,0.809016994374948,0.));
#13187=DIRECTION('',(-0.587785252292472,-0.809016994374948,0.));
#13188=DIRECTION('',(0.,0.,-1.));
#13189=DIRECTION('',(-0.587785252292472,-0.809016994374948,0.));
#13190=DIRECTION('center_axis',(0.,0.,1.));
#13191=DIRECTION('ref_axis',(1.,0.,0.));
#13192=DIRECTION('',(0.809016994374946,-0.587785252292475,0.));
#13193=DIRECTION('center_axis',(0.,0.,1.));
#13194=DIRECTION('ref_axis',(1.,0.,0.));
#13195=DIRECTION('',(0.809016994374946,-0.587785252292475,0.));
#13196=DIRECTION('center_axis',(0.587785252292475,0.809016994374946,0.));
#13197=DIRECTION('ref_axis',(-0.809016994374946,0.587785252292475,0.));
#13198=DIRECTION('center_axis',(-0.587785252292472,0.809016994374948,0.));
#13199=DIRECTION('ref_axis',(-0.809016994374948,-0.587785252292472,0.));
#13200=DIRECTION('',(0.809016994374948,0.587785252292472,0.));
#13201=DIRECTION('',(0.,0.,-1.));
#13202=DIRECTION('',(0.809016994374948,0.587785252292472,0.));
#13203=DIRECTION('center_axis',(0.587785252292472,-0.809016994374948,0.));
#13204=DIRECTION('ref_axis',(0.809016994374948,0.587785252292472,0.));
#13205=DIRECTION('',(-0.809016994374948,-0.587785252292472,0.));
#13206=DIRECTION('',(0.,0.,-1.));
#13207=DIRECTION('',(-0.809016994374948,-0.587785252292472,0.));
#13208=DIRECTION('center_axis',(0.,0.,1.));
#13209=DIRECTION('ref_axis',(1.,0.,0.));
#13210=DIRECTION('',(0.587785252292475,-0.809016994374946,0.));
#13211=DIRECTION('center_axis',(0.,0.,1.));
#13212=DIRECTION('ref_axis',(1.,0.,0.));
#13213=DIRECTION('',(0.587785252292475,-0.809016994374946,0.));
#13214=DIRECTION('center_axis',(0.809016994374946,0.587785252292475,0.));
#13215=DIRECTION('ref_axis',(-0.587785252292475,0.809016994374946,0.));
#13216=DIRECTION('center_axis',(-0.453990499739548,0.891006524188367,0.));
#13217=DIRECTION('ref_axis',(-0.891006524188367,-0.453990499739548,0.));
#13218=DIRECTION('',(0.891006524188367,0.453990499739548,0.));
#13219=DIRECTION('',(0.,0.,-1.));
#13220=DIRECTION('',(0.891006524188367,0.453990499739548,0.));
#13221=DIRECTION('center_axis',(0.453990499739548,-0.891006524188367,0.));
#13222=DIRECTION('ref_axis',(0.891006524188367,0.453990499739548,0.));
#13223=DIRECTION('',(-0.891006524188367,-0.453990499739548,0.));
#13224=DIRECTION('',(0.,0.,-1.));
#13225=DIRECTION('',(-0.891006524188367,-0.453990499739548,0.));
#13226=DIRECTION('center_axis',(0.,0.,1.));
#13227=DIRECTION('ref_axis',(1.,0.,0.));
#13228=DIRECTION('',(0.453990499739554,-0.891006524188364,0.));
#13229=DIRECTION('center_axis',(0.,0.,1.));
#13230=DIRECTION('ref_axis',(1.,0.,0.));
#13231=DIRECTION('',(0.453990499739554,-0.891006524188364,0.));
#13232=DIRECTION('center_axis',(0.891006524188364,0.453990499739554,0.));
#13233=DIRECTION('ref_axis',(-0.453990499739554,0.891006524188364,0.));
#13234=DIRECTION('center_axis',(-0.309016994374947,0.951056516295154,0.));
#13235=DIRECTION('ref_axis',(-0.951056516295154,-0.309016994374947,0.));
#13236=DIRECTION('',(0.951056516295154,0.309016994374947,0.));
#13237=DIRECTION('',(0.,0.,-1.));
#13238=DIRECTION('',(0.951056516295154,0.309016994374947,0.));
#13239=DIRECTION('center_axis',(0.309016994374948,-0.951056516295154,0.));
#13240=DIRECTION('ref_axis',(0.951056516295154,0.309016994374948,0.));
#13241=DIRECTION('',(-0.951056516295153,-0.309016994374948,0.));
#13242=DIRECTION('',(0.,0.,-1.));
#13243=DIRECTION('',(-0.951056516295153,-0.309016994374948,0.));
#13244=DIRECTION('center_axis',(0.,0.,1.));
#13245=DIRECTION('ref_axis',(1.,0.,0.));
#13246=DIRECTION('',(0.309016994374941,-0.951056516295156,0.));
#13247=DIRECTION('center_axis',(0.,0.,1.));
#13248=DIRECTION('ref_axis',(1.,0.,0.));
#13249=DIRECTION('',(0.309016994374941,-0.951056516295156,0.));
#13250=DIRECTION('center_axis',(0.951056516295156,0.309016994374941,0.));
#13251=DIRECTION('ref_axis',(-0.309016994374941,0.951056516295156,0.));
#13252=DIRECTION('axis',(0.,0.,1.));
#13253=DIRECTION('refdir',(1.,0.,0.));
#13254=DIRECTION('center_axis',(0.,0.,-1.));
#13255=DIRECTION('ref_axis',(-1.,0.,0.));
#13256=DIRECTION('center_axis',(0.,0.,1.));
#13257=DIRECTION('ref_axis',(1.,0.,0.));
#13258=DIRECTION('',(0.,0.,-1.));
#13259=DIRECTION('center_axis',(0.,0.,1.));
#13260=DIRECTION('ref_axis',(1.,0.,0.));
#13261=DIRECTION('center_axis',(0.,0.,-1.));
#13262=DIRECTION('ref_axis',(-1.,0.,0.));
#13263=DIRECTION('center_axis',(0.,0.,1.));
#13264=DIRECTION('ref_axis',(1.,0.,0.));
#13265=DIRECTION('',(0.,0.,-1.));
#13266=DIRECTION('center_axis',(0.,0.,1.));
#13267=DIRECTION('ref_axis',(1.,0.,0.));
#13268=DIRECTION('center_axis',(0.,0.,1.));
#13269=DIRECTION('ref_axis',(1.,0.,0.));
#13270=DIRECTION('',(0.,-1.,0.));
#13271=DIRECTION('',(0.64018439966448,-0.768221279597376,0.));
#13272=DIRECTION('',(0.98058067569092,-0.196116135138184,0.));
#13273=DIRECTION('',(0.999512076087079,0.0312347523777212,0.));
#13274=DIRECTION('',(1.,0.,0.));
#13275=DIRECTION('',(0.993883734673619,0.110431526074847,0.));
#13276=DIRECTION('',(0.78086880944303,0.624695047554424,0.));
#13277=DIRECTION('',(0.,1.,0.));
#13278=DIRECTION('',(-0.78086880944303,0.624695047554424,0.));
#13279=DIRECTION('',(-0.993883734673619,0.110431526074847,0.));
#13280=DIRECTION('',(-1.,0.,0.));
#13281=DIRECTION('',(-0.999512076087079,0.0312347523777212,0.));
#13282=DIRECTION('',(-0.98058067569092,-0.196116135138184,0.));
#13283=DIRECTION('',(-0.64018439966448,-0.768221279597376,0.));
#13284=DIRECTION('center_axis',(0.,0.,1.));
#13285=DIRECTION('ref_axis',(1.,0.,0.));
#13286=DIRECTION('',(0.,-1.,0.));
#13287=DIRECTION('',(-0.64018439966448,-0.768221279597376,0.));
#13288=DIRECTION('',(-0.98058067569092,-0.196116135138184,0.));
#13289=DIRECTION('',(-0.999512076087079,0.0312347523777212,0.));
#13290=DIRECTION('',(-1.,0.,0.));
#13291=DIRECTION('',(-0.993883734673619,0.110431526074847,0.));
#13292=DIRECTION('',(-0.78086880944303,0.624695047554424,0.));
#13293=DIRECTION('',(0.,1.,0.));
#13294=DIRECTION('',(0.78086880944303,0.624695047554424,0.));
#13295=DIRECTION('',(0.993883734673619,0.110431526074847,0.));
#13296=DIRECTION('',(1.,0.,0.));
#13297=DIRECTION('',(0.999512076087079,0.0312347523777212,0.));
#13298=DIRECTION('',(0.98058067569092,-0.196116135138184,0.));
#13299=DIRECTION('',(0.64018439966448,-0.768221279597376,0.));
#13300=DIRECTION('center_axis',(1.,0.,0.));
#13301=DIRECTION('ref_axis',(0.,0.,-1.));
#13302=DIRECTION('',(0.,0.,-1.));
#13303=DIRECTION('',(0.,0.,-1.));
#13304=DIRECTION('center_axis',(0.768221279597376,0.64018439966448,0.));
#13305=DIRECTION('ref_axis',(-0.64018439966448,0.768221279597376,0.));
#13306=DIRECTION('',(0.,0.,-1.));
#13307=DIRECTION('center_axis',(0.196116135138184,0.98058067569092,0.));
#13308=DIRECTION('ref_axis',(-0.98058067569092,0.196116135138184,0.));
#13309=DIRECTION('',(0.,0.,-1.));
#13310=DIRECTION('center_axis',(-0.0312347523777212,0.999512076087079,0.));
#13311=DIRECTION('ref_axis',(-0.999512076087079,-0.0312347523777212,0.));
#13312=DIRECTION('',(0.,0.,-1.));
#13313=DIRECTION('center_axis',(0.,1.,0.));
#13314=DIRECTION('ref_axis',(0.,0.,1.));
#13315=DIRECTION('',(0.,0.,-1.));
#13316=DIRECTION('center_axis',(-0.110431526074847,0.993883734673619,0.));
#13317=DIRECTION('ref_axis',(-0.993883734673619,-0.110431526074847,0.));
#13318=DIRECTION('',(0.,0.,-1.));
#13319=DIRECTION('center_axis',(-0.624695047554425,0.78086880944303,0.));
#13320=DIRECTION('ref_axis',(-0.78086880944303,-0.624695047554424,0.));
#13321=DIRECTION('',(0.,0.,-1.));
#13322=DIRECTION('center_axis',(-1.,0.,0.));
#13323=DIRECTION('ref_axis',(0.,0.,1.));
#13324=DIRECTION('',(0.,0.,-1.));
#13325=DIRECTION('center_axis',(-0.624695047554425,-0.78086880944303,0.));
#13326=DIRECTION('ref_axis',(0.78086880944303,-0.624695047554424,0.));
#13327=DIRECTION('',(0.,0.,-1.));
#13328=DIRECTION('center_axis',(-0.110431526074847,-0.993883734673619,0.));
#13329=DIRECTION('ref_axis',(0.993883734673619,-0.110431526074847,0.));
#13330=DIRECTION('',(0.,0.,-1.));
#13331=DIRECTION('center_axis',(0.,-1.,0.));
#13332=DIRECTION('ref_axis',(0.,0.,-1.));
#13333=DIRECTION('',(0.,0.,-1.));
#13334=DIRECTION('center_axis',(-0.0312347523777212,-0.999512076087079,
0.));
#13335=DIRECTION('ref_axis',(0.999512076087079,-0.0312347523777212,0.));
#13336=DIRECTION('',(0.,0.,-1.));
#13337=DIRECTION('center_axis',(0.196116135138184,-0.98058067569092,0.));
#13338=DIRECTION('ref_axis',(0.98058067569092,0.196116135138184,0.));
#13339=DIRECTION('',(0.,0.,-1.));
#13340=DIRECTION('center_axis',(0.768221279597376,-0.64018439966448,0.));
#13341=DIRECTION('ref_axis',(0.64018439966448,0.768221279597376,0.));
#13342=DIRECTION('axis',(0.,0.,1.));
#13343=DIRECTION('refdir',(1.,0.,0.));
#13344=DIRECTION('center_axis',(0.,0.,-1.));
#13345=DIRECTION('ref_axis',(-1.,0.,0.));
#13346=DIRECTION('center_axis',(0.,0.,-1.));
#13347=DIRECTION('ref_axis',(-1.,0.,0.));
#13348=DIRECTION('',(-0.209529088730874,2.56599127842526E-17,0.977802414077409));
#13349=DIRECTION('center_axis',(0.,0.,-1.));
#13350=DIRECTION('ref_axis',(-1.,0.,0.));
#13351=DIRECTION('center_axis',(0.,0.,-1.));
#13352=DIRECTION('ref_axis',(-1.,0.,0.));
#13353=DIRECTION('center_axis',(0.,0.,-1.));
#13354=DIRECTION('ref_axis',(-1.,0.,0.));
#13355=DIRECTION('center_axis',(0.,0.,-1.));
#13356=DIRECTION('ref_axis',(-1.,0.,0.));
#13357=DIRECTION('',(0.,0.,1.));
#13358=DIRECTION('center_axis',(0.,0.,1.));
#13359=DIRECTION('ref_axis',(1.,0.,0.));
#13360=DIRECTION('',(0.447213595499958,5.47678698264203E-17,-0.894427190999916));
#13361=DIRECTION('center_axis',(0.,0.,-1.));
#13362=DIRECTION('ref_axis',(-1.,0.,0.));
#13363=DIRECTION('center_axis',(0.,0.,-1.));
#13364=DIRECTION('ref_axis',(-1.,0.,0.));
#13365=DIRECTION('center_axis',(0.,0.,-1.));
#13366=DIRECTION('ref_axis',(-1.,0.,0.));
#13367=DIRECTION('',(0.,0.,-1.));
#13368=DIRECTION('center_axis',(0.,0.,-1.));
#13369=DIRECTION('ref_axis',(-1.,0.,0.));
#13370=DIRECTION('center_axis',(0.,0.,1.));
#13371=DIRECTION('ref_axis',(1.,0.,0.));
#13372=DIRECTION('center_axis',(0.,0.,-1.));
#13373=DIRECTION('ref_axis',(-1.,0.,0.));
#13374=DIRECTION('axis',(0.,0.,1.));
#13375=DIRECTION('refdir',(1.,0.,0.));
#13376=DIRECTION('center_axis',(0.,0.,-1.));
#13377=DIRECTION('ref_axis',(-1.,0.,0.));
#13378=DIRECTION('center_axis',(0.,0.,1.));
#13379=DIRECTION('ref_axis',(1.,0.,0.));
#13380=DIRECTION('',(0.,0.,1.));
#13381=DIRECTION('center_axis',(0.,0.,1.));
#13382=DIRECTION('ref_axis',(1.,0.,0.));
#13383=DIRECTION('center_axis',(0.,0.,-1.));
#13384=DIRECTION('ref_axis',(-1.,0.,0.));
#13385=DIRECTION('center_axis',(0.,0.,1.));
#13386=DIRECTION('ref_axis',(1.,0.,0.));
#13387=DIRECTION('',(0.,0.,1.));
#13388=DIRECTION('center_axis',(0.,0.,1.));
#13389=DIRECTION('ref_axis',(1.,0.,0.));
#13390=DIRECTION('center_axis',(0.,0.,1.));
#13391=DIRECTION('ref_axis',(1.,0.,0.));
#13392=DIRECTION('center_axis',(0.,0.,1.));
#13393=DIRECTION('ref_axis',(1.,0.,0.));
#13394=DIRECTION('center_axis',(0.,0.,1.));
#13395=DIRECTION('ref_axis',(1.,0.,0.));
#13396=DIRECTION('axis',(0.,0.,1.));
#13397=DIRECTION('refdir',(1.,0.,0.));
#13398=DIRECTION('center_axis',(0.,0.,-1.));
#13399=DIRECTION('ref_axis',(-1.,0.,0.));
#13400=DIRECTION('center_axis',(0.,0.,1.));
#13401=DIRECTION('ref_axis',(1.,0.,0.));
#13402=DIRECTION('',(0.,0.,-1.));
#13403=DIRECTION('center_axis',(0.,0.,1.));
#13404=DIRECTION('ref_axis',(1.,0.,0.));
#13405=DIRECTION('center_axis',(0.,0.,1.));
#13406=DIRECTION('ref_axis',(1.,0.,0.));
#13407=DIRECTION('',(0.5,0.866025403784439,0.));
#13408=DIRECTION('',(-0.5,0.866025403784439,0.));
#13409=DIRECTION('',(-1.,1.1556266144132E-16,0.));
#13410=DIRECTION('',(-0.5,-0.866025403784438,0.));
#13411=DIRECTION('',(0.5,-0.866025403784439,0.));
#13412=DIRECTION('',(1.,-2.3112532288264E-16,0.));
#13413=DIRECTION('center_axis',(0.,0.,1.));
#13414=DIRECTION('ref_axis',(1.,0.,0.));
#13415=DIRECTION('',(0.5,0.866025403784439,0.));
#13416=DIRECTION('',(1.,-2.3112532288264E-16,0.));
#13417=DIRECTION('',(0.5,-0.866025403784439,0.));
#13418=DIRECTION('',(-0.5,-0.866025403784438,0.));
#13419=DIRECTION('',(-1.,1.1556266144132E-16,0.));
#13420=DIRECTION('',(-0.5,0.866025403784439,0.));
#13421=DIRECTION('center_axis',(-0.866025403784439,0.5,0.));
#13422=DIRECTION('ref_axis',(-0.5,-0.866025403784439,0.));
#13423=DIRECTION('',(0.,0.,-1.));
#13424=DIRECTION('',(0.,0.,-1.));
#13425=DIRECTION('center_axis',(-0.866025403784439,-0.5,0.));
#13426=DIRECTION('ref_axis',(0.5,-0.866025403784439,0.));
#13427=DIRECTION('',(0.,0.,-1.));
#13428=DIRECTION('center_axis',(-1.1556266144132E-16,-1.,0.));
#13429=DIRECTION('ref_axis',(1.,-1.1556266144132E-16,0.));
#13430=DIRECTION('',(0.,0.,-1.));
#13431=DIRECTION('center_axis',(0.866025403784439,-0.5,0.));
#13432=DIRECTION('ref_axis',(0.5,0.866025403784439,0.));
#13433=DIRECTION('',(0.,0.,-1.));
#13434=DIRECTION('center_axis',(0.866025403784439,0.5,0.));
#13435=DIRECTION('ref_axis',(-0.5,0.866025403784439,0.));
#13436=DIRECTION('',(0.,0.,-1.));
#13437=DIRECTION('center_axis',(2.3112532288264E-16,1.,0.));
#13438=DIRECTION('ref_axis',(-1.,2.3112532288264E-16,0.));
#13439=DIRECTION('axis',(0.,0.,1.));
#13440=DIRECTION('refdir',(1.,0.,0.));
#13441=DIRECTION('center_axis',(0.,0.,-1.));
#13442=DIRECTION('ref_axis',(-1.,0.,0.));
#13443=DIRECTION('center_axis',(0.,0.,1.));
#13444=DIRECTION('ref_axis',(1.,0.,0.));
#13445=DIRECTION('',(0.,0.,1.));
#13446=DIRECTION('center_axis',(0.,0.,1.));
#13447=DIRECTION('ref_axis',(1.,0.,0.));
#13448=DIRECTION('center_axis',(0.,0.,-1.));
#13449=DIRECTION('ref_axis',(-1.,0.,0.));
#13450=DIRECTION('center_axis',(0.,0.,1.));
#13451=DIRECTION('ref_axis',(1.,0.,0.));
#13452=DIRECTION('',(0.,0.,1.));
#13453=DIRECTION('center_axis',(0.,0.,1.));
#13454=DIRECTION('ref_axis',(1.,0.,0.));
#13455=DIRECTION('center_axis',(0.,0.,1.));
#13456=DIRECTION('ref_axis',(1.,0.,0.));
#13457=DIRECTION('',(-0.5,-0.866025403784438,0.));
#13458=DIRECTION('',(0.5,-0.866025403784438,0.));
#13459=DIRECTION('',(1.,-1.87789324842145E-16,0.));
#13460=DIRECTION('',(0.5,0.866025403784438,0.));
#13461=DIRECTION('',(-0.5,0.866025403784439,0.));
#13462=DIRECTION('',(-1.,0.,0.));
#13463=DIRECTION('center_axis',(0.,0.,1.));
#13464=DIRECTION('ref_axis',(1.,0.,0.));
#13465=DIRECTION('center_axis',(0.,0.,1.));
#13466=DIRECTION('ref_axis',(1.,0.,0.));
#13467=DIRECTION('center_axis',(-0.866025403784439,0.5,0.));
#13468=DIRECTION('ref_axis',(-0.5,-0.866025403784439,0.));
#13469=DIRECTION('',(0.,0.,-1.));
#13470=DIRECTION('',(0.5,0.866025403784439,0.));
#13471=DIRECTION('',(0.,0.,-1.));
#13472=DIRECTION('center_axis',(-0.866025403784439,-0.5,0.));
#13473=DIRECTION('ref_axis',(0.5,-0.866025403784439,0.));
#13474=DIRECTION('',(-0.5,0.866025403784439,0.));
#13475=DIRECTION('',(0.,0.,-1.));
#13476=DIRECTION('center_axis',(-1.87789324842145E-16,-1.,0.));
#13477=DIRECTION('ref_axis',(1.,-1.87789324842145E-16,0.));
#13478=DIRECTION('',(-1.,1.87789324842145E-16,0.));
#13479=DIRECTION('',(0.,0.,-1.));
#13480=DIRECTION('center_axis',(0.866025403784438,-0.5,0.));
#13481=DIRECTION('ref_axis',(0.5,0.866025403784438,0.));
#13482=DIRECTION('',(-0.5,-0.866025403784438,0.));
#13483=DIRECTION('',(0.,0.,-1.));
#13484=DIRECTION('center_axis',(0.866025403784439,0.5,0.));
#13485=DIRECTION('ref_axis',(-0.5,0.866025403784439,0.));
#13486=DIRECTION('',(0.5,-0.866025403784439,0.));
#13487=DIRECTION('',(0.,0.,-1.));
#13488=DIRECTION('center_axis',(0.,1.,0.));
#13489=DIRECTION('ref_axis',(0.,0.,1.));
#13490=DIRECTION('',(1.,0.,0.));
#13491=DIRECTION('center_axis',(0.,0.,1.));
#13492=DIRECTION('ref_axis',(1.,0.,0.));
#13493=DIRECTION('axis',(0.,0.,1.));
#13494=DIRECTION('refdir',(1.,0.,0.));
#13495=DIRECTION('center_axis',(0.,0.,-1.));
#13496=DIRECTION('ref_axis',(-1.,0.,0.));
#13497=DIRECTION('center_axis',(0.,0.,1.));
#13498=DIRECTION('ref_axis',(1.,0.,0.));
#13499=DIRECTION('',(0.,0.,1.));
#13500=DIRECTION('center_axis',(0.,0.,1.));
#13501=DIRECTION('ref_axis',(1.,0.,0.));
#13502=DIRECTION('center_axis',(-0.866025403784439,0.5,0.));
#13503=DIRECTION('ref_axis',(-0.5,-0.866025403784439,0.));
#13504=DIRECTION('',(0.5,0.866025403784439,0.));
#13505=DIRECTION('',(0.,0.,-1.));
#13506=DIRECTION('',(0.5,0.866025403784439,0.));
#13507=DIRECTION('',(0.,0.,-1.));
#13508=DIRECTION('center_axis',(-0.866025403784439,-0.5,0.));
#13509=DIRECTION('ref_axis',(0.5,-0.866025403784439,0.));
#13510=DIRECTION('',(-0.5,0.866025403784439,0.));
#13511=DIRECTION('',(0.,0.,-1.));
#13512=DIRECTION('',(-0.5,0.866025403784439,0.));
#13513=DIRECTION('center_axis',(-1.87789324842145E-16,-1.,0.));
#13514=DIRECTION('ref_axis',(1.,-1.87789324842145E-16,0.));
#13515=DIRECTION('',(-1.,1.87789324842145E-16,0.));
#13516=DIRECTION('',(0.,0.,-1.));
#13517=DIRECTION('',(-1.,1.87789324842145E-16,0.));
#13518=DIRECTION('center_axis',(0.866025403784438,-0.5,0.));
#13519=DIRECTION('ref_axis',(0.5,0.866025403784438,0.));
#13520=DIRECTION('',(-0.5,-0.866025403784438,0.));
#13521=DIRECTION('',(0.,0.,-1.));
#13522=DIRECTION('',(-0.5,-0.866025403784438,0.));
#13523=DIRECTION('center_axis',(0.866025403784439,0.5,0.));
#13524=DIRECTION('ref_axis',(-0.5,0.866025403784439,0.));
#13525=DIRECTION('',(0.5,-0.866025403784439,0.));
#13526=DIRECTION('',(0.,0.,-1.));
#13527=DIRECTION('',(0.5,-0.866025403784439,0.));
#13528=DIRECTION('center_axis',(0.,1.,0.));
#13529=DIRECTION('ref_axis',(0.,0.,1.));
#13530=DIRECTION('',(1.,0.,0.));
#13531=DIRECTION('',(1.,0.,0.));
#13532=DIRECTION('center_axis',(0.,0.,1.));
#13533=DIRECTION('ref_axis',(1.,0.,0.));
#13534=DIRECTION('center_axis',(0.,0.,1.));
#13535=DIRECTION('ref_axis',(1.,0.,0.));
#13536=DIRECTION('center_axis',(0.,0.,1.));
#13537=DIRECTION('ref_axis',(1.,0.,0.));
#13538=DIRECTION('axis',(0.,0.,1.));
#13539=DIRECTION('refdir',(1.,0.,0.));
#13540=DIRECTION('center_axis',(0.,0.,-1.));
#13541=DIRECTION('ref_axis',(-1.,0.,0.));
#13542=DIRECTION('center_axis',(0.,0.,1.));
#13543=DIRECTION('ref_axis',(1.,0.,0.));
#13544=DIRECTION('',(0.,0.,1.));
#13545=DIRECTION('center_axis',(0.,0.,1.));
#13546=DIRECTION('ref_axis',(1.,0.,0.));
#13547=DIRECTION('center_axis',(0.,0.,-1.));
#13548=DIRECTION('ref_axis',(-1.,0.,0.));
#13549=DIRECTION('center_axis',(0.,0.,1.));
#13550=DIRECTION('ref_axis',(1.,0.,0.));
#13551=DIRECTION('',(0.,0.,1.));
#13552=DIRECTION('center_axis',(0.,0.,1.));
#13553=DIRECTION('ref_axis',(1.,0.,0.));
#13554=DIRECTION('center_axis',(0.,0.,1.));
#13555=DIRECTION('ref_axis',(1.,0.,0.));
#13556=DIRECTION('',(-0.5,-0.866025403784439,0.));
#13557=DIRECTION('',(0.5,-0.866025403784439,0.));
#13558=DIRECTION('',(1.,-1.50231459873716E-16,0.));
#13559=DIRECTION('',(0.5,0.866025403784438,0.));
#13560=DIRECTION('',(-0.5,0.866025403784439,0.));
#13561=DIRECTION('',(-1.,1.50231459873716E-16,0.));
#13562=DIRECTION('center_axis',(0.,0.,1.));
#13563=DIRECTION('ref_axis',(1.,0.,0.));
#13564=DIRECTION('center_axis',(0.,0.,1.));
#13565=DIRECTION('ref_axis',(1.,0.,0.));
#13566=DIRECTION('center_axis',(-0.866025403784439,0.5,0.));
#13567=DIRECTION('ref_axis',(-0.5,-0.866025403784439,0.));
#13568=DIRECTION('',(0.,0.,-1.));
#13569=DIRECTION('',(0.5,0.866025403784439,0.));
#13570=DIRECTION('',(0.,0.,-1.));
#13571=DIRECTION('center_axis',(-0.866025403784439,-0.5,0.));
#13572=DIRECTION('ref_axis',(0.5,-0.866025403784439,0.));
#13573=DIRECTION('',(-0.5,0.866025403784439,0.));
#13574=DIRECTION('',(0.,0.,-1.));
#13575=DIRECTION('center_axis',(-1.50231459873716E-16,-1.,0.));
#13576=DIRECTION('ref_axis',(1.,-1.50231459873716E-16,0.));
#13577=DIRECTION('',(-1.,1.50231459873716E-16,0.));
#13578=DIRECTION('',(0.,0.,-1.));
#13579=DIRECTION('center_axis',(0.866025403784439,-0.5,0.));
#13580=DIRECTION('ref_axis',(0.5,0.866025403784439,0.));
#13581=DIRECTION('',(-0.5,-0.866025403784438,0.));
#13582=DIRECTION('',(0.,0.,-1.));
#13583=DIRECTION('center_axis',(0.866025403784439,0.5,0.));
#13584=DIRECTION('ref_axis',(-0.5,0.866025403784439,0.));
#13585=DIRECTION('',(0.5,-0.866025403784439,0.));
#13586=DIRECTION('',(0.,0.,-1.));
#13587=DIRECTION('center_axis',(1.50231459873716E-16,1.,0.));
#13588=DIRECTION('ref_axis',(-1.,1.50231459873716E-16,0.));
#13589=DIRECTION('',(1.,-1.50231459873716E-16,0.));
#13590=DIRECTION('center_axis',(0.,0.,1.));
#13591=DIRECTION('ref_axis',(1.,0.,0.));
#13592=DIRECTION('',(0.,0.,1.));
#13593=DIRECTION('',(1.,0.,0.));
#13594=DIRECTION('',(0.,0.,1.));
#13595=DIRECTION('',(1.,0.,0.));
#13596=DIRECTION('',(0.,0.,1.));
#13597=DIRECTION('',(1.,0.,0.));
#13598=DIRECTION('',(0.,0.,1.));
#13599=DIRECTION('',(1.,0.,0.));
#13600=DIRECTION('',(0.,0.,1.));
#13601=DIRECTION('',(1.,0.,0.));
#13602=DIRECTION('',(0.,0.,1.));
#13603=DIRECTION('',(1.,0.,0.));
#13604=DIRECTION('',(0.,0.,1.));
#13605=DIRECTION('',(1.,0.,0.));
#13606=DIRECTION('',(0.,0.,1.));
#13607=DIRECTION('',(1.,0.,0.));
#13608=DIRECTION('',(1.,0.,0.));
#13609=DIRECTION('',(0.,1.,0.));
#13610=DIRECTION('',(1.,0.,0.));
#13611=DIRECTION('',(0.,1.,0.));
#13612=DIRECTION('',(0.,-1.,0.));
#13613=DIRECTION('',(-1.,0.,0.));
#13614=DIRECTION('',(0.,1.,0.));
#13615=DIRECTION('',(1.,0.,0.));
#13616=DIRECTION('',(0.,0.,1.));
#13617=DIRECTION('',(1.,0.,0.));
#13618=DIRECTION('',(0.,0.,1.));
#13619=DIRECTION('',(1.,0.,0.));
#13620=DIRECTION('',(1.,0.,0.));
#13621=DIRECTION('',(0.,1.,0.));
#13622=DIRECTION('',(1.,0.,0.));
#13623=DIRECTION('',(0.,1.,0.));
#13624=DIRECTION('',(-1.,0.,0.));
#13625=DIRECTION('',(0.,1.,0.));
#13626=DIRECTION('',(0.,0.,1.));
#13627=DIRECTION('',(1.,0.,0.));
#13628=DIRECTION('',(-1.,0.,0.));
#13629=DIRECTION('',(0.,1.,0.));
#13630=DIRECTION('',(1.,0.,0.));
#13631=DIRECTION('',(0.,1.,0.));
#13632=DIRECTION('',(1.,0.,0.));
#13633=DIRECTION('',(0.,1.,0.));
#13634=DIRECTION('',(0.,1.,0.));
#13635=DIRECTION('',(1.,0.,0.));
#13636=DIRECTION('',(0.,-1.,0.));
#13637=DIRECTION('',(1.,0.,0.));
#13638=DIRECTION('',(0.,0.,1.));
#13639=DIRECTION('',(1.,0.,0.));
#13640=DIRECTION('',(0.,0.,-1.));
#13641=DIRECTION('',(1.,0.,0.));
#13642=DIRECTION('',(0.,1.,0.));
#13643=DIRECTION('',(-1.,0.,0.));
#13644=DIRECTION('',(0.,-1.,0.));
#13645=DIRECTION('',(-1.,0.,0.));
#13646=DIRECTION('',(0.,-1.,0.));
#13647=DIRECTION('',(-1.,0.,0.));
#13648=DIRECTION('',(0.,1.,0.));
#13649=DIRECTION('',(-1.,0.,0.));
#13650=DIRECTION('',(0.,1.,0.));
#13651=DIRECTION('',(-1.,0.,0.));
#13652=DIRECTION('',(0.,-1.,0.));
#13653=DIRECTION('',(-1.,0.,0.));
#13654=DIRECTION('',(0.,-1.,0.));
#13655=DIRECTION('',(1.,0.,0.));
#13656=DIRECTION('',(0.,1.,0.));
#13657=DIRECTION('',(1.,0.,0.));
#13658=DIRECTION('',(0.,-1.,0.));
#13659=DIRECTION('',(1.,0.,0.));
#13660=DIRECTION('',(1.,0.,0.));
#13661=DIRECTION('',(0.,1.,0.));
#13662=DIRECTION('',(0.,-1.,0.));
#13663=DIRECTION('',(-1.,0.,0.));
#13664=DIRECTION('',(1.,0.,0.));
#13665=DIRECTION('',(0.,1.,0.));
#13666=DIRECTION('',(0.,-1.,0.));
#13667=DIRECTION('',(-1.,0.,0.));
#13668=DIRECTION('',(0.,-1.,0.));
#13669=DIRECTION('',(1.,0.,0.));
#13670=DIRECTION('',(0.,-1.,0.));
#13671=DIRECTION('',(1.,0.,0.));
#13672=DIRECTION('',(-1.,0.,0.));
#13673=DIRECTION('',(0.,1.,0.));
#13674=DIRECTION('',(-1.,0.,0.));
#13675=DIRECTION('',(0.,1.,0.));
#13676=DIRECTION('',(-1.,0.,0.));
#13677=DIRECTION('',(0.,1.,0.));
#13678=DIRECTION('',(0.,0.,1.));
#13679=DIRECTION('',(1.,0.,0.));
#13680=CARTESIAN_POINT('',(0.,0.,0.));
#13681=CARTESIAN_POINT('',(0.,0.,0.));
#13682=CARTESIAN_POINT('Origin',(-107.,-28.,24.));
#13683=CARTESIAN_POINT('',(-107.,-28.,21.5));
#13684=CARTESIAN_POINT('Origin',(-107.,-28.,24.));
#13685=CARTESIAN_POINT('',(-120.,-28.,21.5));
#13686=CARTESIAN_POINT('',(-107.,-28.,21.5));
#13687=CARTESIAN_POINT('Origin',(-120.,-28.,24.));
#13688=CARTESIAN_POINT('Origin',(-107.,28.,24.));
#13689=CARTESIAN_POINT('',(-107.,28.,21.5));
#13690=CARTESIAN_POINT('Origin',(-107.,28.,24.));
#13691=CARTESIAN_POINT('',(-120.,28.,21.5));
#13692=CARTESIAN_POINT('',(-107.,28.,21.5));
#13693=CARTESIAN_POINT('Origin',(-120.,28.,24.));
#13694=CARTESIAN_POINT('Origin',(0.,0.,8.));
#13695=CARTESIAN_POINT('',(-133.35,-5.71314274283428,8.));
#13696=CARTESIAN_POINT('',(-127.,-5.71314274283428,8.));
#13697=CARTESIAN_POINT('',(-127.,-5.71314274283428,8.));
#13698=CARTESIAN_POINT('',(-133.35,-63.5,8.));
#13699=CARTESIAN_POINT('',(-133.35,-63.5,8.));
#13700=CARTESIAN_POINT('',(-101.,-63.5,8.));
#13701=CARTESIAN_POINT('',(-133.35,-63.5,8.));
#13702=CARTESIAN_POINT('',(-101.,-51.,8.));
#13703=CARTESIAN_POINT('',(-101.,0.,8.));
#13704=CARTESIAN_POINT('',(-89.,-51.,8.));
#13705=CARTESIAN_POINT('',(0.,-51.,8.));
#13706=CARTESIAN_POINT('',(-89.,-63.5,8.));
#13707=CARTESIAN_POINT('',(-89.,0.,8.));
#13708=CARTESIAN_POINT('',(-6.00000000000001,-63.5,8.));
#13709=CARTESIAN_POINT('',(-133.35,-63.5,8.));
#13710=CARTESIAN_POINT('',(-6.,-51.,8.));
#13711=CARTESIAN_POINT('',(-6.,0.,8.));
#13712=CARTESIAN_POINT('',(6.,-51.,8.));
#13713=CARTESIAN_POINT('',(0.,-51.,8.));
#13714=CARTESIAN_POINT('',(6.00000000000001,-63.5,8.));
#13715=CARTESIAN_POINT('',(6.,0.,8.));
#13716=CARTESIAN_POINT('',(89.,-63.5,8.));
#13717=CARTESIAN_POINT('',(-133.35,-63.5,8.));
#13718=CARTESIAN_POINT('',(89.,-51.,8.));
#13719=CARTESIAN_POINT('',(89.,0.,8.));
#13720=CARTESIAN_POINT('',(101.,-51.,8.));
#13721=CARTESIAN_POINT('',(0.,-51.,8.));
#13722=CARTESIAN_POINT('',(101.,-63.5,8.));
#13723=CARTESIAN_POINT('',(101.,0.,8.));
#13724=CARTESIAN_POINT('',(133.35,-63.5,8.));
#13725=CARTESIAN_POINT('',(-133.35,-63.5,8.));
#13726=CARTESIAN_POINT('',(133.35,63.5,8.));
#13727=CARTESIAN_POINT('',(133.35,-63.5,8.));
#13728=CARTESIAN_POINT('',(101.,63.5,8.));
#13729=CARTESIAN_POINT('',(-133.35,63.5,8.));
#13730=CARTESIAN_POINT('',(101.,51.,8.));
#13731=CARTESIAN_POINT('',(101.,0.,8.));
#13732=CARTESIAN_POINT('',(89.,51.,8.));
#13733=CARTESIAN_POINT('',(0.,51.,8.));
#13734=CARTESIAN_POINT('',(89.,63.5,8.));
#13735=CARTESIAN_POINT('',(89.,0.,8.));
#13736=CARTESIAN_POINT('',(6.00000000000001,63.5,8.));
#13737=CARTESIAN_POINT('',(-133.35,63.5,8.));
#13738=CARTESIAN_POINT('',(6.,51.,8.));
#13739=CARTESIAN_POINT('',(6.,0.,8.));
#13740=CARTESIAN_POINT('',(-6.,51.,8.));
#13741=CARTESIAN_POINT('',(0.,51.,8.));
#13742=CARTESIAN_POINT('',(-6.00000000000001,63.5,8.));
#13743=CARTESIAN_POINT('',(-6.,0.,8.));
#13744=CARTESIAN_POINT('',(-89.,63.5,8.));
#13745=CARTESIAN_POINT('',(-133.35,63.5,8.));
#13746=CARTESIAN_POINT('',(-89.,51.,8.));
#13747=CARTESIAN_POINT('',(-89.,0.,8.));
#13748=CARTESIAN_POINT('',(-101.,51.,8.));
#13749=CARTESIAN_POINT('',(0.,51.,8.));
#13750=CARTESIAN_POINT('',(-101.,63.5,8.));
#13751=CARTESIAN_POINT('',(-101.,0.,8.));
#13752=CARTESIAN_POINT('',(-133.35,63.5,8.));
#13753=CARTESIAN_POINT('',(-133.35,63.5,8.));
#13754=CARTESIAN_POINT('',(-133.35,5.71314274283428,8.));
#13755=CARTESIAN_POINT('',(-133.35,-63.5,8.));
#13756=CARTESIAN_POINT('',(-127.,5.71314274283428,8.));
#13757=CARTESIAN_POINT('',(-127.,5.71314274283428,8.));
#13758=CARTESIAN_POINT('',(-127.,0.,8.));
#13759=CARTESIAN_POINT('',(120.,12.,8.));
#13760=CARTESIAN_POINT('',(120.,33.,8.));
#13761=CARTESIAN_POINT('',(120.,33.,8.));
#13762=CARTESIAN_POINT('',(-120.,12.,8.));
#13763=CARTESIAN_POINT('',(120.,12.,8.));
#13764=CARTESIAN_POINT('',(-120.,33.,8.));
#13765=CARTESIAN_POINT('',(-120.,33.,8.));
#13766=CARTESIAN_POINT('',(120.,33.,8.));
#13767=CARTESIAN_POINT('',(120.,-12.,8.));
#13768=CARTESIAN_POINT('',(-120.,-12.,8.));
#13769=CARTESIAN_POINT('',(120.,-12.,8.));
#13770=CARTESIAN_POINT('',(120.,-33.,8.));
#13771=CARTESIAN_POINT('',(120.,-33.,8.));
#13772=CARTESIAN_POINT('',(-120.,-33.,8.));
#13773=CARTESIAN_POINT('',(120.,-33.,8.));
#13774=CARTESIAN_POINT('',(-120.,-33.,8.));
#13775=CARTESIAN_POINT('Origin',(-133.35,63.5,8.));
#13776=CARTESIAN_POINT('',(6.,63.5,0.));
#13777=CARTESIAN_POINT('',(6.00000000000001,63.5,8.));
#13778=CARTESIAN_POINT('',(89.,63.5,0.));
#13779=CARTESIAN_POINT('',(89.,63.5,8.));
#13780=CARTESIAN_POINT('',(-133.35,63.5,0.));
#13781=CARTESIAN_POINT('Origin',(-133.35,63.5,8.));
#13782=CARTESIAN_POINT('',(-6.,63.5,0.));
#13783=CARTESIAN_POINT('',(-6.00000000000001,63.5,8.));
#13784=CARTESIAN_POINT('',(-89.,63.5,0.));
#13785=CARTESIAN_POINT('',(-133.35,63.5,0.));
#13786=CARTESIAN_POINT('',(-89.,63.5,8.));
#13787=CARTESIAN_POINT('Origin',(-133.35,63.5,8.));
#13788=CARTESIAN_POINT('',(-101.,63.5,0.));
#13789=CARTESIAN_POINT('',(-101.,63.5,8.));
#13790=CARTESIAN_POINT('',(-133.35,63.5,0.));
#13791=CARTESIAN_POINT('',(-133.35,63.5,0.));
#13792=CARTESIAN_POINT('',(-133.35,63.5,8.));
#13793=CARTESIAN_POINT('Origin',(-133.35,63.5,8.));
#13794=CARTESIAN_POINT('',(101.,63.5,0.));
#13795=CARTESIAN_POINT('',(101.,63.5,8.));
#13796=CARTESIAN_POINT('',(133.35,63.5,0.));
#13797=CARTESIAN_POINT('',(133.35,63.5,8.));
#13798=CARTESIAN_POINT('',(-133.35,63.5,0.));
#13799=CARTESIAN_POINT('Origin',(-133.35,-63.5,8.));
#13800=CARTESIAN_POINT('',(101.,-63.5,0.));
#13801=CARTESIAN_POINT('',(101.,-63.5,8.));
#13802=CARTESIAN_POINT('',(133.35,-63.5,0.));
#13803=CARTESIAN_POINT('',(-133.35,-63.5,0.));
#13804=CARTESIAN_POINT('',(133.35,-63.5,8.));
#13805=CARTESIAN_POINT('Origin',(-133.35,-63.5,8.));
#13806=CARTESIAN_POINT('',(89.,-63.5,0.));
#13807=CARTESIAN_POINT('',(89.,-63.5,8.));
#13808=CARTESIAN_POINT('',(6.,-63.5,0.));
#13809=CARTESIAN_POINT('',(6.00000000000001,-63.5,8.));
#13810=CARTESIAN_POINT('',(-133.35,-63.5,0.));
#13811=CARTESIAN_POINT('Origin',(-133.35,-63.5,8.));
#13812=CARTESIAN_POINT('',(-6.00000000000001,-63.5,0.));
#13813=CARTESIAN_POINT('',(-6.00000000000001,-63.5,8.));
#13814=CARTESIAN_POINT('',(-89.,-63.5,0.));
#13815=CARTESIAN_POINT('',(-89.,-63.5,8.));
#13816=CARTESIAN_POINT('',(-133.35,-63.5,0.));
#13817=CARTESIAN_POINT('Origin',(-133.35,-63.5,8.));
#13818=CARTESIAN_POINT('',(-101.,-63.5,0.));
#13819=CARTESIAN_POINT('',(-101.,-63.5,8.));
#13820=CARTESIAN_POINT('',(-133.35,-63.5,0.));
#13821=CARTESIAN_POINT('',(-133.35,-63.5,8.));
#13822=CARTESIAN_POINT('',(-133.35,-63.5,0.));
#13823=CARTESIAN_POINT('Origin',(0.,0.,0.));
#13824=CARTESIAN_POINT('',(101.,-51.,0.));
#13825=CARTESIAN_POINT('',(101.,0.,0.));
#13826=CARTESIAN_POINT('',(89.,-51.,0.));
#13827=CARTESIAN_POINT('',(0.,-51.,0.));
#13828=CARTESIAN_POINT('',(89.,0.,0.));
#13829=CARTESIAN_POINT('',(6.,-51.,0.));
#13830=CARTESIAN_POINT('',(6.,0.,0.));
#13831=CARTESIAN_POINT('',(-6.,-51.,0.));
#13832=CARTESIAN_POINT('',(0.,-51.,0.));
#13833=CARTESIAN_POINT('',(-6.,0.,0.));
#13834=CARTESIAN_POINT('',(-89.,-51.,0.));
#13835=CARTESIAN_POINT('',(-89.,0.,0.));
#13836=CARTESIAN_POINT('',(-101.,-51.,0.));
#13837=CARTESIAN_POINT('',(0.,-51.,0.));
#13838=CARTESIAN_POINT('',(-101.,0.,0.));
#13839=CARTESIAN_POINT('',(-133.35,-63.5,0.));
#13840=CARTESIAN_POINT('',(-101.,51.,0.));
#13841=CARTESIAN_POINT('',(-101.,0.,0.));
#13842=CARTESIAN_POINT('',(-89.,51.,0.));
#13843=CARTESIAN_POINT('',(0.,51.,0.));
#13844=CARTESIAN_POINT('',(-89.,0.,0.));
#13845=CARTESIAN_POINT('',(-6.,51.,0.));
#13846=CARTESIAN_POINT('',(-6.,0.,0.));
#13847=CARTESIAN_POINT('',(6.,51.,0.));
#13848=CARTESIAN_POINT('',(0.,51.,0.));
#13849=CARTESIAN_POINT('',(6.,0.,0.));
#13850=CARTESIAN_POINT('',(89.,51.,0.));
#13851=CARTESIAN_POINT('',(89.,0.,0.));
#13852=CARTESIAN_POINT('',(101.,51.,0.));
#13853=CARTESIAN_POINT('',(0.,51.,0.));
#13854=CARTESIAN_POINT('',(101.,0.,0.));
#13855=CARTESIAN_POINT('',(133.35,-63.5,0.));
#13856=CARTESIAN_POINT('Origin',(133.35,-63.5,8.));
#13857=CARTESIAN_POINT('Origin',(-133.35,-63.5,8.));
#13858=CARTESIAN_POINT('Origin',(-133.35,0.,21.));
#13859=CARTESIAN_POINT('Origin',(120.,-33.,16.));
#13860=CARTESIAN_POINT('',(-120.,-33.,16.));
#13861=CARTESIAN_POINT('',(-120.,-33.,16.));
#13862=CARTESIAN_POINT('',(120.,-33.,16.));
#13863=CARTESIAN_POINT('',(120.,-33.,16.));
#13864=CARTESIAN_POINT('',(120.,-33.,16.));
#13865=CARTESIAN_POINT('Origin',(120.,-12.,8.));
#13866=CARTESIAN_POINT('',(-120.,-12.,34.));
#13867=CARTESIAN_POINT('',(-120.,-12.,8.));
#13868=CARTESIAN_POINT('',(120.,-12.,34.));
#13869=CARTESIAN_POINT('',(120.,-12.,34.));
#13870=CARTESIAN_POINT('',(120.,-12.,8.));
#13871=CARTESIAN_POINT('Origin',(120.,-12.,34.));
#13872=CARTESIAN_POINT('',(-120.,-45.,34.));
#13873=CARTESIAN_POINT('',(-120.,-12.,34.));
#13874=CARTESIAN_POINT('',(120.,-45.,34.));
#13875=CARTESIAN_POINT('',(120.,-45.,34.));
#13876=CARTESIAN_POINT('',(120.,-12.,34.));
#13877=CARTESIAN_POINT('Origin',(120.,-45.,34.));
#13878=CARTESIAN_POINT('',(-120.,-45.,34.));
#13879=CARTESIAN_POINT('',(120.,-45.,34.));
#13880=CARTESIAN_POINT('Origin',(120.,0.,0.));
#13881=CARTESIAN_POINT('Origin',(-120.,0.,0.));
#13882=CARTESIAN_POINT('Origin',(120.,33.,16.));
#13883=CARTESIAN_POINT('',(-120.,33.,16.));
#13884=CARTESIAN_POINT('',(-120.,33.,16.));
#13885=CARTESIAN_POINT('',(120.,33.,16.));
#13886=CARTESIAN_POINT('',(120.,33.,16.));
#13887=CARTESIAN_POINT('',(120.,33.,16.));
#13888=CARTESIAN_POINT('Origin',(120.,45.,34.));
#13889=CARTESIAN_POINT('',(-120.,45.,34.));
#13890=CARTESIAN_POINT('',(-120.,45.,34.));
#13891=CARTESIAN_POINT('',(120.,45.,34.));
#13892=CARTESIAN_POINT('',(120.,45.,34.));
#13893=CARTESIAN_POINT('',(120.,45.,34.));
#13894=CARTESIAN_POINT('Origin',(120.,12.,34.));
#13895=CARTESIAN_POINT('',(-120.,12.,34.));
#13896=CARTESIAN_POINT('',(-120.,12.,34.));
#13897=CARTESIAN_POINT('',(120.,12.,34.));
#13898=CARTESIAN_POINT('',(120.,12.,34.));
#13899=CARTESIAN_POINT('',(120.,12.,34.));
#13900=CARTESIAN_POINT('Origin',(120.,12.,8.));
#13901=CARTESIAN_POINT('',(-120.,12.,8.));
#13902=CARTESIAN_POINT('',(120.,12.,8.));
#13903=CARTESIAN_POINT('Origin',(120.,0.,0.));
#13904=CARTESIAN_POINT('Origin',(-120.,0.,0.));
#13905=CARTESIAN_POINT('Origin',(-89.,-71.,9.));
#13906=CARTESIAN_POINT('',(-89.,-51.,9.));
#13907=CARTESIAN_POINT('Origin',(-101.,-51.,9.));
#13908=CARTESIAN_POINT('',(-101.,-51.,9.));
#13909=CARTESIAN_POINT('Origin',(-101.,-71.,9.));
#13910=CARTESIAN_POINT('Origin',(101.,51.,9.));
#13911=CARTESIAN_POINT('',(101.,51.,9.));
#13912=CARTESIAN_POINT('Origin',(89.,51.,9.));
#13913=CARTESIAN_POINT('',(89.,51.,9.));
#13914=CARTESIAN_POINT('Origin',(89.,51.,9.));
#13915=CARTESIAN_POINT('Origin',(-89.,51.,9.));
#13916=CARTESIAN_POINT('',(-89.,51.,9.));
#13917=CARTESIAN_POINT('Origin',(-101.,51.,9.));
#13918=CARTESIAN_POINT('',(-101.,51.,9.));
#13919=CARTESIAN_POINT('Origin',(-101.,51.,9.));
#13920=CARTESIAN_POINT('Origin',(6.,-71.,9.));
#13921=CARTESIAN_POINT('',(6.,-51.,9.));
#13922=CARTESIAN_POINT('Origin',(-6.,-51.,9.));
#13923=CARTESIAN_POINT('',(-6.,-51.,9.));
#13924=CARTESIAN_POINT('Origin',(-6.,-71.,9.));
#13925=CARTESIAN_POINT('Origin',(6.,51.,9.));
#13926=CARTESIAN_POINT('',(6.,51.,9.));
#13927=CARTESIAN_POINT('Origin',(-6.,51.,9.));
#13928=CARTESIAN_POINT('',(-6.,51.,9.));
#13929=CARTESIAN_POINT('Origin',(-6.,51.,9.));
#13930=CARTESIAN_POINT('Origin',(101.,-71.,9.));
#13931=CARTESIAN_POINT('',(101.,-51.,9.));
#13932=CARTESIAN_POINT('Origin',(89.,-51.,9.));
#13933=CARTESIAN_POINT('',(89.,-51.,9.));
#13934=CARTESIAN_POINT('Origin',(89.,-71.,9.));
#13935=CARTESIAN_POINT('Origin',(-107.,28.,24.));
#13936=CARTESIAN_POINT('Origin',(-107.,-28.,24.));
#13937=CARTESIAN_POINT('Origin',(-127.,0.,21.));
#13938=CARTESIAN_POINT('Origin',(-127.,0.,21.));
#13939=CARTESIAN_POINT('Origin',(-127.,0.,21.));
#13940=CARTESIAN_POINT('',(0.,0.,0.));
#13941=CARTESIAN_POINT('Origin',(0.,111.,55.));
#13942=CARTESIAN_POINT('',(8.97997772825745,110.,44.));
#13943=CARTESIAN_POINT('',(-8.97997772825745,110.,44.));
#13944=CARTESIAN_POINT('Origin',(0.,110.,55.));
#13945=CARTESIAN_POINT('',(-8.97997772825745,107.,44.));
#13946=CARTESIAN_POINT('',(-8.97997772825745,111.,44.));
#13947=CARTESIAN_POINT('',(8.97997772825745,107.,44.));
#13948=CARTESIAN_POINT('Origin',(0.,107.,55.));
#13949=CARTESIAN_POINT('',(8.97997772825745,111.,44.));
#13950=CARTESIAN_POINT('Origin',(-28.,101.,58.));
#13951=CARTESIAN_POINT('',(-28.,100.,60.5));
#13952=CARTESIAN_POINT('Origin',(-28.,100.,58.));
#13953=CARTESIAN_POINT('',(-28.,87.,60.5));
#13954=CARTESIAN_POINT('',(-28.,101.,60.5));
#13955=CARTESIAN_POINT('Origin',(-28.,87.,58.));
#13956=CARTESIAN_POINT('Origin',(28.,101.,58.));
#13957=CARTESIAN_POINT('',(28.,100.,60.5));
#13958=CARTESIAN_POINT('Origin',(28.,100.,58.));
#13959=CARTESIAN_POINT('',(28.,87.,60.5));
#13960=CARTESIAN_POINT('',(28.,101.,60.5));
#13961=CARTESIAN_POINT('Origin',(28.,87.,58.));
#13962=CARTESIAN_POINT('Origin',(-45.,58.,26.));
#13963=CARTESIAN_POINT('',(-45.,56.,28.6));
#13964=CARTESIAN_POINT('Origin',(-45.,56.,26.));
#13965=CARTESIAN_POINT('',(-45.,44.85,28.6));
#13966=CARTESIAN_POINT('',(-45.,58.,28.6));
#13967=CARTESIAN_POINT('',(-47.5941038915202,43.,25.825));
#13968=CARTESIAN_POINT('Origin',(-45.0000000000008,43.1166666666671,26.0000000000007));
#13969=CARTESIAN_POINT('',(-42.4058961084799,43.,25.825));
#13970=CARTESIAN_POINT('Origin',(-45.,43.,26.));
#13971=CARTESIAN_POINT('Origin',(-45.0000000000008,43.1166666666671,26.0000000000007));
#13972=CARTESIAN_POINT('Origin',(0.,58.,26.));
#13973=CARTESIAN_POINT('',(-3.18408167778312E-16,56.,28.6));
#13974=CARTESIAN_POINT('Origin',(0.,56.,26.));
#13975=CARTESIAN_POINT('',(-3.18408167778385E-16,44.85,28.6));
#13976=CARTESIAN_POINT('',(-3.18408167778312E-16,58.,28.6));
#13977=CARTESIAN_POINT('',(-2.59410389152015,43.,25.825));
#13978=CARTESIAN_POINT('Origin',(-2.41519961368208E-13,43.1166666666668,
26.0000000000002));
#13979=CARTESIAN_POINT('',(2.59410389152015,43.,25.825));
#13980=CARTESIAN_POINT('Origin',(0.,43.,26.));
#13981=CARTESIAN_POINT('Origin',(-2.41519961368208E-13,43.1166666666668,
26.0000000000002));
#13982=CARTESIAN_POINT('Origin',(45.,58.,26.));
#13983=CARTESIAN_POINT('',(45.,56.,28.6));
#13984=CARTESIAN_POINT('Origin',(45.,56.,26.));
#13985=CARTESIAN_POINT('',(45.,44.85,28.6));
#13986=CARTESIAN_POINT('',(45.,58.,28.6));
#13987=CARTESIAN_POINT('',(42.4058961084799,43.,25.825));
#13988=CARTESIAN_POINT('Origin',(45.,43.1166666666666,25.9999999999999));
#13989=CARTESIAN_POINT('',(47.5941038915202,43.,25.825));
#13990=CARTESIAN_POINT('Origin',(45.,43.,26.));
#13991=CARTESIAN_POINT('Origin',(45.,43.1166666666666,25.9999999999999));
#13992=CARTESIAN_POINT('Origin',(68.,110.,44.));
#13993=CARTESIAN_POINT('',(68.,107.,44.));
#13994=CARTESIAN_POINT('',(-68.,110.,44.));
#13995=CARTESIAN_POINT('',(68.,110.,44.));
#13996=CARTESIAN_POINT('',(-68.,-110.,44.));
#13997=CARTESIAN_POINT('',(-68.,110.,44.));
#13998=CARTESIAN_POINT('',(68.,-110.,44.));
#13999=CARTESIAN_POINT('',(68.,-110.,44.));
#14000=CARTESIAN_POINT('',(68.,110.,44.));
#14001=CARTESIAN_POINT('',(68.,110.,44.));
#14002=CARTESIAN_POINT('',(68.,110.,44.));
#14003=CARTESIAN_POINT('',(-12.,100.,44.));
#14004=CARTESIAN_POINT('',(-33.,100.,44.));
#14005=CARTESIAN_POINT('',(-33.,100.,44.));
#14006=CARTESIAN_POINT('',(-12.,-100.,44.));
#14007=CARTESIAN_POINT('',(-12.,100.,44.));
#14008=CARTESIAN_POINT('',(-33.,-100.,44.));
#14009=CARTESIAN_POINT('',(-33.,-100.,44.));
#14010=CARTESIAN_POINT('',(-33.,100.,44.));
#14011=CARTESIAN_POINT('',(12.,100.,44.));
#14012=CARTESIAN_POINT('',(12.,-100.,44.));
#14013=CARTESIAN_POINT('',(12.,100.,44.));
#14014=CARTESIAN_POINT('',(33.,100.,44.));
#14015=CARTESIAN_POINT('',(33.,100.,44.));
#14016=CARTESIAN_POINT('',(33.,-100.,44.));
#14017=CARTESIAN_POINT('',(33.,100.,44.));
#14018=CARTESIAN_POINT('',(33.,-100.,44.));
#14019=CARTESIAN_POINT('Origin',(68.,48.65,34.3));
#14020=CARTESIAN_POINT('',(-68.,48.65,34.3));
#14021=CARTESIAN_POINT('',(-68.,36.65,16.3));
#14022=CARTESIAN_POINT('',(-68.,48.65,34.3));
#14023=CARTESIAN_POINT('',(68.,36.65,16.3));
#14024=CARTESIAN_POINT('',(68.,36.65,16.3));
#14025=CARTESIAN_POINT('',(68.,48.65,34.3));
#14026=CARTESIAN_POINT('',(68.,48.65,34.3));
#14027=CARTESIAN_POINT('',(68.,48.65,34.3));
#14028=CARTESIAN_POINT('',(68.,43.,25.825));
#14029=CARTESIAN_POINT('',(68.,43.,25.825));
#14030=CARTESIAN_POINT('',(68.,43.,25.825));
#14031=CARTESIAN_POINT('Origin',(68.,-110.,44.));
#14032=CARTESIAN_POINT('',(-68.,-110.,36.));
#14033=CARTESIAN_POINT('',(-68.,-110.,44.));
#14034=CARTESIAN_POINT('',(68.,-110.,36.));
#14035=CARTESIAN_POINT('',(68.,-110.,36.));
#14036=CARTESIAN_POINT('',(68.,-110.,44.));
#14037=CARTESIAN_POINT('Origin',(68.,-110.,36.));
#14038=CARTESIAN_POINT('',(-68.,-56.,36.));
#14039=CARTESIAN_POINT('',(-68.,-110.,36.));
#14040=CARTESIAN_POINT('',(68.,-56.,36.));
#14041=CARTESIAN_POINT('',(68.,-56.,36.));
#14042=CARTESIAN_POINT('',(68.,-110.,36.));
#14043=CARTESIAN_POINT('Origin',(68.,-56.,36.));
#14044=CARTESIAN_POINT('',(-68.,-56.,16.3));
#14045=CARTESIAN_POINT('',(-68.,-56.,36.));
#14046=CARTESIAN_POINT('',(68.,-56.,16.3));
#14047=CARTESIAN_POINT('',(68.,-56.,16.3));
#14048=CARTESIAN_POINT('',(68.,-56.,36.));
#14049=CARTESIAN_POINT('Origin',(68.,-56.,16.3));
#14050=CARTESIAN_POINT('',(-68.,-33.45,16.3));
#14051=CARTESIAN_POINT('',(-68.,-56.,16.3));
#14052=CARTESIAN_POINT('',(68.,-33.45,16.3));
#14053=CARTESIAN_POINT('',(68.,-33.45,16.3));
#14054=CARTESIAN_POINT('',(68.,-56.,16.3));
#14055=CARTESIAN_POINT('Origin',(68.,-33.45,16.3));
#14056=CARTESIAN_POINT('',(-68.,-45.45,34.3));
#14057=CARTESIAN_POINT('',(-68.,-33.45,16.3));
#14058=CARTESIAN_POINT('',(68.,-45.45,34.3));
#14059=CARTESIAN_POINT('',(68.,-45.45,34.3));
#14060=CARTESIAN_POINT('',(68.,-33.45,16.3));
#14061=CARTESIAN_POINT('Origin',(68.,-45.45,34.3));
#14062=CARTESIAN_POINT('',(-68.,-45.45,34.3));
#14063=CARTESIAN_POINT('',(68.,-45.45,34.3));
#14064=CARTESIAN_POINT('Origin',(68.,36.65,16.3));
#14065=CARTESIAN_POINT('',(-68.,56.,16.3));
#14066=CARTESIAN_POINT('',(-68.,36.65,16.3));
#14067=CARTESIAN_POINT('',(68.,56.,16.3));
#14068=CARTESIAN_POINT('',(68.,56.,16.3));
#14069=CARTESIAN_POINT('',(68.,36.65,16.3));
#14070=CARTESIAN_POINT('Origin',(68.,56.,16.3));
#14071=CARTESIAN_POINT('',(-68.,56.,36.));
#14072=CARTESIAN_POINT('',(-68.,56.,16.3));
#14073=CARTESIAN_POINT('',(68.,56.,36.));
#14074=CARTESIAN_POINT('',(68.,56.,36.));
#14075=CARTESIAN_POINT('',(68.,56.,16.3));
#14076=CARTESIAN_POINT('Origin',(68.,56.,36.));
#14077=CARTESIAN_POINT('',(-68.,110.,36.));
#14078=CARTESIAN_POINT('',(-68.,56.,36.));
#14079=CARTESIAN_POINT('',(68.,110.,36.));
#14080=CARTESIAN_POINT('',(68.,110.,36.));
#14081=CARTESIAN_POINT('',(68.,56.,36.));
#14082=CARTESIAN_POINT('Origin',(68.,110.,36.));
#14083=CARTESIAN_POINT('',(68.,110.,36.));
#14084=CARTESIAN_POINT('',(-68.,110.,36.));
#14085=CARTESIAN_POINT('Origin',(68.,0.,0.));
#14086=CARTESIAN_POINT('Origin',(-68.,0.,0.));
#14087=CARTESIAN_POINT('Origin',(-33.,100.,50.));
#14088=CARTESIAN_POINT('',(-33.,-100.,50.));
#14089=CARTESIAN_POINT('',(-33.,-100.,50.));
#14090=CARTESIAN_POINT('',(-33.,100.,50.));
#14091=CARTESIAN_POINT('',(-33.,100.,50.));
#14092=CARTESIAN_POINT('',(-33.,100.,50.));
#14093=CARTESIAN_POINT('Origin',(-45.,100.,68.));
#14094=CARTESIAN_POINT('',(-45.,-100.,68.));
#14095=CARTESIAN_POINT('',(-45.,-100.,68.));
#14096=CARTESIAN_POINT('',(-45.,100.,68.));
#14097=CARTESIAN_POINT('',(-45.,100.,68.));
#14098=CARTESIAN_POINT('',(-45.,100.,68.));
#14099=CARTESIAN_POINT('Origin',(-12.,100.,68.));
#14100=CARTESIAN_POINT('',(-12.,-100.,68.));
#14101=CARTESIAN_POINT('',(-12.,-100.,68.));
#14102=CARTESIAN_POINT('',(-12.,100.,68.));
#14103=CARTESIAN_POINT('',(-12.,100.,68.));
#14104=CARTESIAN_POINT('',(-12.,100.,68.));
#14105=CARTESIAN_POINT('Origin',(-12.,100.,44.));
#14106=CARTESIAN_POINT('',(-12.,-100.,44.));
#14107=CARTESIAN_POINT('',(-12.,100.,44.));
#14108=CARTESIAN_POINT('Origin',(0.,100.,0.));
#14109=CARTESIAN_POINT('Origin',(0.,-100.,0.));
#14110=CARTESIAN_POINT('Origin',(33.,100.,50.));
#14111=CARTESIAN_POINT('',(33.,-100.,50.));
#14112=CARTESIAN_POINT('',(33.,-100.,50.));
#14113=CARTESIAN_POINT('',(33.,100.,50.));
#14114=CARTESIAN_POINT('',(33.,100.,50.));
#14115=CARTESIAN_POINT('',(33.,100.,50.));
#14116=CARTESIAN_POINT('Origin',(12.,100.,44.));
#14117=CARTESIAN_POINT('',(12.,-100.,68.));
#14118=CARTESIAN_POINT('',(12.,-100.,44.));
#14119=CARTESIAN_POINT('',(12.,100.,68.));
#14120=CARTESIAN_POINT('',(12.,100.,68.));
#14121=CARTESIAN_POINT('',(12.,100.,44.));
#14122=CARTESIAN_POINT('Origin',(12.,100.,68.));
#14123=CARTESIAN_POINT('',(45.,-100.,68.));
#14124=CARTESIAN_POINT('',(12.,-100.,68.));
#14125=CARTESIAN_POINT('',(45.,100.,68.));
#14126=CARTESIAN_POINT('',(45.,100.,68.));
#14127=CARTESIAN_POINT('',(12.,100.,68.));
#14128=CARTESIAN_POINT('Origin',(45.,100.,68.));
#14129=CARTESIAN_POINT('',(45.,-100.,68.));
#14130=CARTESIAN_POINT('',(45.,100.,68.));
#14131=CARTESIAN_POINT('Origin',(0.,100.,0.));
#14132=CARTESIAN_POINT('Origin',(0.,-100.,0.));
#14133=CARTESIAN_POINT('Origin',(45.,43.,26.));
#14134=CARTESIAN_POINT('Origin',(0.,43.,26.));
#14135=CARTESIAN_POINT('Origin',(-45.,43.,26.));
#14136=CARTESIAN_POINT('Origin',(28.,87.,58.));
#14137=CARTESIAN_POINT('Origin',(-28.,87.,58.));
#14138=CARTESIAN_POINT('Origin',(0.,107.,55.));
#14139=CARTESIAN_POINT('',(0.,0.,0.));
#14140=CARTESIAN_POINT('Origin',(58.,-36.,60.));
#14141=CARTESIAN_POINT('',(56.,-36.,57.4));
#14142=CARTESIAN_POINT('Origin',(56.,-36.,60.));
#14143=CARTESIAN_POINT('',(43.,-36.,57.4));
#14144=CARTESIAN_POINT('',(58.,-36.,57.4));
#14145=CARTESIAN_POINT('',(43.,-38.5941038915202,59.825));
#14146=CARTESIAN_POINT('Origin',(43.,-36.,60.));
#14147=CARTESIAN_POINT('',(43.,-33.4058961084799,59.825));
#14148=CARTESIAN_POINT('Origin',(43.1166666666667,-36.0000000000003,60.0000000000001));
#14149=CARTESIAN_POINT('Origin',(43.,-36.,60.));
#14150=CARTESIAN_POINT('Origin',(58.,0.,60.));
#14151=CARTESIAN_POINT('',(56.,-3.18408167778311E-16,57.4));
#14152=CARTESIAN_POINT('Origin',(56.,0.,60.));
#14153=CARTESIAN_POINT('',(43.,-3.18408167778311E-16,57.4));
#14154=CARTESIAN_POINT('',(58.,-3.18408167778311E-16,57.4));
#14155=CARTESIAN_POINT('',(43.,-2.59410389152015,59.825));
#14156=CARTESIAN_POINT('Origin',(43.,0.,60.));
#14157=CARTESIAN_POINT('',(43.,2.59410389152015,59.825));
#14158=CARTESIAN_POINT('Origin',(43.1166666666672,-9.08717545655691E-13,
60.0000000000008));
#14159=CARTESIAN_POINT('Origin',(43.,0.,60.));
#14160=CARTESIAN_POINT('Origin',(58.,36.,60.));
#14161=CARTESIAN_POINT('',(56.,36.,57.4));
#14162=CARTESIAN_POINT('Origin',(56.,36.,60.));
#14163=CARTESIAN_POINT('',(43.,36.,57.4));
#14164=CARTESIAN_POINT('',(58.,36.,57.4));
#14165=CARTESIAN_POINT('',(43.,33.4058961084799,59.825));
#14166=CARTESIAN_POINT('Origin',(43.,36.,60.));
#14167=CARTESIAN_POINT('',(43.,38.5941038915202,59.825));
#14168=CARTESIAN_POINT('Origin',(43.1166666666669,35.9999999999995,60.0000000000004));
#14169=CARTESIAN_POINT('Origin',(43.,36.,60.));
#14170=CARTESIAN_POINT('Origin',(-32.,97.,115.8875));
#14171=CARTESIAN_POINT('',(-32.,97.,118.3875));
#14172=CARTESIAN_POINT('Origin',(-32.,97.,115.8875));
#14173=CARTESIAN_POINT('',(-32.,82.,118.3875));
#14174=CARTESIAN_POINT('',(-32.,97.,118.3875));
#14175=CARTESIAN_POINT('Origin',(-32.,82.,115.8875));
#14176=CARTESIAN_POINT('Origin',(32.,97.,115.8875));
#14177=CARTESIAN_POINT('',(32.,97.,118.3875));
#14178=CARTESIAN_POINT('Origin',(32.,97.,115.8875));
#14179=CARTESIAN_POINT('',(32.,82.,118.3875));
#14180=CARTESIAN_POINT('',(32.,97.,118.3875));
#14181=CARTESIAN_POINT('Origin',(32.,82.,115.8875));
#14182=CARTESIAN_POINT('Origin',(0.,-86.,113.));
#14183=CARTESIAN_POINT('',(-1.11442858722409E-15,-87.,122.1));
#14184=CARTESIAN_POINT('Origin',(0.,-87.,113.));
#14185=CARTESIAN_POINT('',(-1.11442858722409E-15,-105.,122.1));
#14186=CARTESIAN_POINT('',(-1.11442858722409E-15,-86.,122.1));
#14187=CARTESIAN_POINT('Origin',(0.,-105.,113.));
#14188=CARTESIAN_POINT('Origin',(56.,49.,82.));
#14189=CARTESIAN_POINT('',(-22.,-87.,82.));
#14190=CARTESIAN_POINT('',(-22.,-105.,82.));
#14191=CARTESIAN_POINT('',(-22.,-87.,82.));
#14192=CARTESIAN_POINT('',(22.,-87.,82.));
#14193=CARTESIAN_POINT('',(-22.,-87.,82.));
#14194=CARTESIAN_POINT('',(22.,-105.,82.));
#14195=CARTESIAN_POINT('',(22.,-87.,82.));
#14196=CARTESIAN_POINT('',(56.,-105.,82.));
#14197=CARTESIAN_POINT('',(-56.,-105.,82.));
#14198=CARTESIAN_POINT('',(56.,105.,82.));
#14199=CARTESIAN_POINT('',(56.,49.,82.));
#14200=CARTESIAN_POINT('',(50.8,105.,82.));
#14201=CARTESIAN_POINT('',(-56.,105.,82.));
#14202=CARTESIAN_POINT('',(50.8,82.,82.));
#14203=CARTESIAN_POINT('',(50.8,105.,82.));
#14204=CARTESIAN_POINT('',(-50.8,82.,82.));
#14205=CARTESIAN_POINT('',(-50.8,82.,82.));
#14206=CARTESIAN_POINT('',(-50.8,105.,82.));
#14207=CARTESIAN_POINT('',(-50.8,105.,82.));
#14208=CARTESIAN_POINT('',(-56.,105.,82.));
#14209=CARTESIAN_POINT('',(-56.,105.,82.));
#14210=CARTESIAN_POINT('',(-56.,-105.,82.));
#14211=CARTESIAN_POINT('',(-56.,49.,82.));
#14212=CARTESIAN_POINT('',(-56.,-105.,82.));
#14213=CARTESIAN_POINT('',(8.,-79.,82.));
#14214=CARTESIAN_POINT('',(16.,-79.,82.));
#14215=CARTESIAN_POINT('',(56.,-79.,82.));
#14216=CARTESIAN_POINT('',(8.,-80.,82.));
#14217=CARTESIAN_POINT('',(8.,49.,82.));
#14218=CARTESIAN_POINT('',(-8.,-80.,82.));
#14219=CARTESIAN_POINT('',(56.,-80.,82.));
#14220=CARTESIAN_POINT('',(-8.,-79.,82.));
#14221=CARTESIAN_POINT('',(-8.,49.,82.));
#14222=CARTESIAN_POINT('',(-16.,-79.,82.));
#14223=CARTESIAN_POINT('',(56.,-79.,82.));
#14224=CARTESIAN_POINT('',(-16.,-47.,82.));
#14225=CARTESIAN_POINT('',(-16.,49.,82.));
#14226=CARTESIAN_POINT('',(-8.,-47.,82.));
#14227=CARTESIAN_POINT('',(56.,-47.,82.));
#14228=CARTESIAN_POINT('',(-8.,76.,82.));
#14229=CARTESIAN_POINT('',(-8.,49.,82.));
#14230=CARTESIAN_POINT('',(8.,76.,82.));
#14231=CARTESIAN_POINT('',(56.,76.,82.));
#14232=CARTESIAN_POINT('',(8.,-47.,82.));
#14233=CARTESIAN_POINT('',(8.,49.,82.));
#14234=CARTESIAN_POINT('',(16.,-47.,82.));
#14235=CARTESIAN_POINT('',(56.,-47.,82.));
#14236=CARTESIAN_POINT('',(16.,49.,82.));
#14237=CARTESIAN_POINT('Origin',(0.,-49.,0.));
#14238=CARTESIAN_POINT('',(16.,-49.,69.));
#14239=CARTESIAN_POINT('',(-16.,-49.,69.));
#14240=CARTESIAN_POINT('',(0.,-49.,69.));
#14241=CARTESIAN_POINT('',(-16.,-49.,70.));
#14242=CARTESIAN_POINT('',(-16.,-49.,0.));
#14243=CARTESIAN_POINT('',(-56.,-49.,70.));
#14244=CARTESIAN_POINT('',(0.,-49.,70.));
#14245=CARTESIAN_POINT('',(-56.,-49.,50.3));
#14246=CARTESIAN_POINT('',(-56.,-49.,82.));
#14247=CARTESIAN_POINT('',(-33.45,-49.,50.3));
#14248=CARTESIAN_POINT('',(-56.,-49.,50.3));
#14249=CARTESIAN_POINT('',(-45.45,-49.,68.3));
#14250=CARTESIAN_POINT('',(-33.45,-49.,50.3));
#14251=CARTESIAN_POINT('',(48.65,-49.,68.3));
#14252=CARTESIAN_POINT('',(-45.45,-49.,68.3));
#14253=CARTESIAN_POINT('',(36.65,-49.,50.3));
#14254=CARTESIAN_POINT('',(48.65,-49.,68.3));
#14255=CARTESIAN_POINT('',(56.,-49.,50.3));
#14256=CARTESIAN_POINT('',(36.65,-49.,50.3));
#14257=CARTESIAN_POINT('',(56.,-49.,70.));
#14258=CARTESIAN_POINT('',(56.,-49.,50.3));
#14259=CARTESIAN_POINT('',(16.,-49.,70.));
#14260=CARTESIAN_POINT('',(0.,-49.,70.));
#14261=CARTESIAN_POINT('',(16.,-49.,0.));
#14262=CARTESIAN_POINT('Origin',(0.,0.,70.));
#14263=CARTESIAN_POINT('',(-16.,-79.,70.));
#14264=CARTESIAN_POINT('',(-16.,0.,70.));
#14265=CARTESIAN_POINT('',(16.,-79.,70.));
#14266=CARTESIAN_POINT('',(0.,-79.,70.));
#14267=CARTESIAN_POINT('',(16.,0.,70.));
#14268=CARTESIAN_POINT('',(56.,-105.,70.));
#14269=CARTESIAN_POINT('',(56.,-105.,70.));
#14270=CARTESIAN_POINT('',(-56.,-105.,70.));
#14271=CARTESIAN_POINT('',(-56.,-105.,70.));
#14272=CARTESIAN_POINT('',(-56.,-105.,70.));
#14273=CARTESIAN_POINT('Origin',(8.,76.,78.));
#14274=CARTESIAN_POINT('',(8.,-79.,78.));
#14275=CARTESIAN_POINT('',(8.,-79.,78.));
#14276=CARTESIAN_POINT('',(8.,-80.,78.));
#14277=CARTESIAN_POINT('',(8.,76.,78.));
#14278=CARTESIAN_POINT('',(8.,-80.,78.));
#14279=CARTESIAN_POINT('Origin',(8.,76.,78.));
#14280=CARTESIAN_POINT('',(8.,76.,78.));
#14281=CARTESIAN_POINT('',(8.,-47.,78.));
#14282=CARTESIAN_POINT('',(8.,76.,78.));
#14283=CARTESIAN_POINT('',(8.,-47.,78.));
#14284=CARTESIAN_POINT('',(8.,76.,78.));
#14285=CARTESIAN_POINT('Origin',(-8.,76.,83.));
#14286=CARTESIAN_POINT('',(-8.,-79.,78.));
#14287=CARTESIAN_POINT('',(-8.,-80.,78.));
#14288=CARTESIAN_POINT('',(-8.,76.,78.));
#14289=CARTESIAN_POINT('',(-8.,-79.,83.));
#14290=CARTESIAN_POINT('',(-8.,-80.,83.));
#14291=CARTESIAN_POINT('Origin',(-8.,76.,83.));
#14292=CARTESIAN_POINT('',(-8.,-47.,78.));
#14293=CARTESIAN_POINT('',(-8.,-47.,83.));
#14294=CARTESIAN_POINT('',(-8.,76.,78.));
#14295=CARTESIAN_POINT('',(-8.,76.,78.));
#14296=CARTESIAN_POINT('',(-8.,76.,83.));
#14297=CARTESIAN_POINT('Origin',(16.,76.,78.));
#14298=CARTESIAN_POINT('',(16.,-79.,78.));
#14299=CARTESIAN_POINT('',(16.,-79.,78.));
#14300=CARTESIAN_POINT('',(16.,-80.,78.));
#14301=CARTESIAN_POINT('',(16.,76.,78.));
#14302=CARTESIAN_POINT('',(16.,-80.,78.));
#14303=CARTESIAN_POINT('Origin',(16.,76.,78.));
#14304=CARTESIAN_POINT('',(16.,76.,78.));
#14305=CARTESIAN_POINT('',(16.,-47.,78.));
#14306=CARTESIAN_POINT('',(16.,76.,78.));
#14307=CARTESIAN_POINT('',(16.,-47.,78.));
#14308=CARTESIAN_POINT('',(16.,76.,78.));
#14309=CARTESIAN_POINT('Origin',(-16.,76.,72.));
#14310=CARTESIAN_POINT('',(16.,-79.,72.));
#14311=CARTESIAN_POINT('',(16.,-80.,72.));
#14312=CARTESIAN_POINT('',(16.,76.,72.));
#14313=CARTESIAN_POINT('',(-16.,-79.,72.));
#14314=CARTESIAN_POINT('',(-16.,-79.,72.));
#14315=CARTESIAN_POINT('',(-16.,-80.,72.));
#14316=CARTESIAN_POINT('',(-16.,76.,72.));
#14317=CARTESIAN_POINT('',(-16.,-80.,72.));
#14318=CARTESIAN_POINT('Origin',(-16.,76.,72.));
#14319=CARTESIAN_POINT('',(-16.,76.,72.));
#14320=CARTESIAN_POINT('',(-16.,-47.,72.));
#14321=CARTESIAN_POINT('',(-16.,76.,72.));
#14322=CARTESIAN_POINT('',(16.,-47.,72.));
#14323=CARTESIAN_POINT('',(-16.,-47.,72.));
#14324=CARTESIAN_POINT('',(16.,76.,72.));
#14325=CARTESIAN_POINT('',(16.,76.,72.));
#14326=CARTESIAN_POINT('',(-16.,76.,72.));
#14327=CARTESIAN_POINT('Origin',(-8.,76.,78.));
#14328=CARTESIAN_POINT('',(-16.,-79.,78.));
#14329=CARTESIAN_POINT('',(-16.,-80.,78.));
#14330=CARTESIAN_POINT('',(-16.,76.,78.));
#14331=CARTESIAN_POINT('',(-8.,-79.,78.));
#14332=CARTESIAN_POINT('',(-8.,-80.,78.));
#14333=CARTESIAN_POINT('Origin',(-8.,76.,78.));
#14334=CARTESIAN_POINT('',(-16.,-47.,78.));
#14335=CARTESIAN_POINT('',(-8.,-47.,78.));
#14336=CARTESIAN_POINT('',(-16.,76.,78.));
#14337=CARTESIAN_POINT('',(-16.,76.,78.));
#14338=CARTESIAN_POINT('',(-8.,76.,78.));
#14339=CARTESIAN_POINT('Origin',(48.65,49.,68.3));
#14340=CARTESIAN_POINT('',(48.65,49.,68.3));
#14341=CARTESIAN_POINT('',(48.65,49.,68.3));
#14342=CARTESIAN_POINT('',(36.65,49.,50.3));
#14343=CARTESIAN_POINT('',(48.65,49.,68.3));
#14344=CARTESIAN_POINT('',(36.65,49.,50.3));
#14345=CARTESIAN_POINT('',(43.,49.,59.825));
#14346=CARTESIAN_POINT('',(43.,49.,59.825));
#14347=CARTESIAN_POINT('',(43.,49.,59.825));
#14348=CARTESIAN_POINT('Origin',(56.,49.,50.3));
#14349=CARTESIAN_POINT('',(56.,49.,70.));
#14350=CARTESIAN_POINT('',(56.,49.,50.3));
#14351=CARTESIAN_POINT('',(56.,49.,50.3));
#14352=CARTESIAN_POINT('',(56.,105.,70.));
#14353=CARTESIAN_POINT('',(56.,-105.,70.));
#14354=CARTESIAN_POINT('',(56.,105.,82.));
#14355=CARTESIAN_POINT('',(56.,-105.,82.));
#14356=CARTESIAN_POINT('',(56.,49.,50.3));
#14357=CARTESIAN_POINT('Origin',(36.65,49.,50.3));
#14358=CARTESIAN_POINT('',(36.65,49.,50.3));
#14359=CARTESIAN_POINT('Origin',(-45.45,49.,68.3));
#14360=CARTESIAN_POINT('',(-45.45,49.,68.3));
#14361=CARTESIAN_POINT('',(-45.45,49.,68.3));
#14362=CARTESIAN_POINT('',(-45.45,49.,68.3));
#14363=CARTESIAN_POINT('Origin',(-33.45,49.,50.3));
#14364=CARTESIAN_POINT('',(-33.45,49.,50.3));
#14365=CARTESIAN_POINT('',(-33.45,49.,50.3));
#14366=CARTESIAN_POINT('',(-33.45,49.,50.3));
#14367=CARTESIAN_POINT('Origin',(-56.,49.,50.3));
#14368=CARTESIAN_POINT('',(-56.,49.,50.3));
#14369=CARTESIAN_POINT('',(-56.,49.,50.3));
#14370=CARTESIAN_POINT('',(-56.,49.,50.3));
#14371=CARTESIAN_POINT('Origin',(-56.,49.,82.));
#14372=CARTESIAN_POINT('',(-56.,-105.,82.));
#14373=CARTESIAN_POINT('',(-56.,105.,70.));
#14374=CARTESIAN_POINT('',(-56.,105.,82.));
#14375=CARTESIAN_POINT('',(-56.,49.,70.));
#14376=CARTESIAN_POINT('',(-56.,-105.,70.));
#14377=CARTESIAN_POINT('',(-56.,49.,82.));
#14378=CARTESIAN_POINT('Origin',(0.,49.,0.));
#14379=CARTESIAN_POINT('',(0.,49.,70.));
#14380=CARTESIAN_POINT('Origin',(-56.,-105.,82.));
#14381=CARTESIAN_POINT('',(22.,-105.,119.));
#14382=CARTESIAN_POINT('',(22.,-105.,82.));
#14383=CARTESIAN_POINT('',(12.0000000000003,-105.,129.));
#14384=CARTESIAN_POINT('',(22.,-105.,119.));
#14385=CARTESIAN_POINT('',(-12.,-105.,129.));
#14386=CARTESIAN_POINT('',(12.0000000000003,-105.,129.));
#14387=CARTESIAN_POINT('',(-22.,-105.,119.000000000001));
#14388=CARTESIAN_POINT('',(-12.,-105.,129.));
#14389=CARTESIAN_POINT('',(-22.,-105.,119.000000000001));
#14390=CARTESIAN_POINT('Origin',(0.,0.,70.));
#14391=CARTESIAN_POINT('',(-56.,105.,70.));
#14392=CARTESIAN_POINT('Origin',(-56.,105.,82.));
#14393=CARTESIAN_POINT('',(-50.8,105.,127.35));
#14394=CARTESIAN_POINT('',(-50.8,105.,127.35));
#14395=CARTESIAN_POINT('',(-44.8,105.,133.35));
#14396=CARTESIAN_POINT('',(-44.8,105.,133.35));
#14397=CARTESIAN_POINT('',(44.8000000000001,105.,133.35));
#14398=CARTESIAN_POINT('',(44.8000000000001,105.,133.35));
#14399=CARTESIAN_POINT('',(50.8,105.,127.35));
#14400=CARTESIAN_POINT('',(50.8,105.,127.35));
#14401=CARTESIAN_POINT('',(50.8,105.,82.));
#14402=CARTESIAN_POINT('Origin',(-50.8,105.,127.35));
#14403=CARTESIAN_POINT('',(-50.8,82.,127.35));
#14404=CARTESIAN_POINT('',(-50.8,82.,127.35));
#14405=CARTESIAN_POINT('',(-50.8,105.,127.35));
#14406=CARTESIAN_POINT('Origin',(-44.8,105.,133.35));
#14407=CARTESIAN_POINT('',(-44.8,82.,133.35));
#14408=CARTESIAN_POINT('',(-44.8,82.,133.35));
#14409=CARTESIAN_POINT('',(-44.8,105.,133.35));
#14410=CARTESIAN_POINT('Origin',(44.8000000000001,105.,133.35));
#14411=CARTESIAN_POINT('',(44.8000000000001,82.,133.35));
#14412=CARTESIAN_POINT('',(44.8000000000001,82.,133.35));
#14413=CARTESIAN_POINT('',(44.8000000000001,105.,133.35));
#14414=CARTESIAN_POINT('Origin',(50.8,105.,127.35));
#14415=CARTESIAN_POINT('',(50.8,82.,127.35));
#14416=CARTESIAN_POINT('',(50.8,82.,127.35));
#14417=CARTESIAN_POINT('',(50.8,105.,127.35));
#14418=CARTESIAN_POINT('Origin',(50.8,105.,82.));
#14419=CARTESIAN_POINT('',(50.8,82.,82.));
#14420=CARTESIAN_POINT('Origin',(0.,82.,0.));
#14421=CARTESIAN_POINT('Origin',(-22.,-87.,119.000000000001));
#14422=CARTESIAN_POINT('',(-22.,-87.,119.000000000001));
#14423=CARTESIAN_POINT('',(-22.,-87.,119.000000000001));
#14424=CARTESIAN_POINT('',(-22.,-87.,119.000000000001));
#14425=CARTESIAN_POINT('Origin',(-12.,-87.,129.));
#14426=CARTESIAN_POINT('',(-12.,-87.,129.));
#14427=CARTESIAN_POINT('',(-12.,-87.,129.));
#14428=CARTESIAN_POINT('',(-12.,-87.,129.));
#14429=CARTESIAN_POINT('Origin',(12.0000000000003,-87.,129.));
#14430=CARTESIAN_POINT('',(12.0000000000003,-87.,129.));
#14431=CARTESIAN_POINT('',(12.0000000000003,-87.,129.));
#14432=CARTESIAN_POINT('',(12.0000000000003,-87.,129.));
#14433=CARTESIAN_POINT('Origin',(22.,-87.,119.));
#14434=CARTESIAN_POINT('',(22.,-87.,119.));
#14435=CARTESIAN_POINT('',(22.,-87.,119.));
#14436=CARTESIAN_POINT('',(22.,-87.,119.));
#14437=CARTESIAN_POINT('Origin',(22.,-87.,82.));
#14438=CARTESIAN_POINT('',(22.,-87.,82.));
#14439=CARTESIAN_POINT('Origin',(0.,-87.,0.));
#14440=CARTESIAN_POINT('Origin',(0.,76.,0.));
#14441=CARTESIAN_POINT('',(-16.,76.,78.));
#14442=CARTESIAN_POINT('',(16.,76.,72.));
#14443=CARTESIAN_POINT('Origin',(0.,-80.,0.));
#14444=CARTESIAN_POINT('',(16.,-80.,72.));
#14445=CARTESIAN_POINT('',(-16.,-80.,78.));
#14446=CARTESIAN_POINT('Origin',(16.,76.,72.));
#14447=CARTESIAN_POINT('',(16.,-79.,83.));
#14448=CARTESIAN_POINT('',(16.,-79.,83.));
#14449=CARTESIAN_POINT('',(16.,-47.,83.));
#14450=CARTESIAN_POINT('',(16.,-47.,69.));
#14451=CARTESIAN_POINT('',(16.,-47.,83.));
#14452=CARTESIAN_POINT('',(16.,-79.,69.));
#14453=CARTESIAN_POINT('Origin',(-16.,76.,78.));
#14454=CARTESIAN_POINT('',(-16.,-79.,83.));
#14455=CARTESIAN_POINT('',(-16.,-79.,83.));
#14456=CARTESIAN_POINT('',(-16.,-47.,69.));
#14457=CARTESIAN_POINT('',(-16.,-47.,69.));
#14458=CARTESIAN_POINT('',(-16.,-47.,83.));
#14459=CARTESIAN_POINT('',(-16.,-47.,83.));
#14460=CARTESIAN_POINT('Origin',(32.,97.,115.8875));
#14461=CARTESIAN_POINT('Origin',(-32.,97.,115.8875));
#14462=CARTESIAN_POINT('Origin',(43.,36.,60.));
#14463=CARTESIAN_POINT('Origin',(43.,0.,60.));
#14464=CARTESIAN_POINT('Origin',(43.,-36.,60.));
#14465=CARTESIAN_POINT('Origin',(-16.,-79.,83.));
#14466=CARTESIAN_POINT('Origin',(16.,-47.,83.));
#14467=CARTESIAN_POINT('Origin',(16.,-47.,83.));
#14468=CARTESIAN_POINT('',(16.,-47.,69.));
#14469=CARTESIAN_POINT('Origin',(-16.,-79.,83.));
#14470=CARTESIAN_POINT('Origin',(0.,0.,69.));
#14471=CARTESIAN_POINT('Origin',(-16.,-79.,83.));
#14472=CARTESIAN_POINT('Origin',(16.,-47.,83.));
#14473=CARTESIAN_POINT('',(0.,0.,0.));
#14474=CARTESIAN_POINT('Origin',(0.,5.,87.6));
#14475=CARTESIAN_POINT('',(1.65,5.,87.6));
#14476=CARTESIAN_POINT('Origin',(0.,5.,87.6));
#14477=CARTESIAN_POINT('',(1.65,5.,77.7));
#14478=CARTESIAN_POINT('',(1.65,5.,87.6));
#14479=CARTESIAN_POINT('Origin',(0.,5.,77.7));
#14480=CARTESIAN_POINT('Origin',(0.,18.,87.6));
#14481=CARTESIAN_POINT('',(1.65,18.,87.6));
#14482=CARTESIAN_POINT('Origin',(0.,18.,87.6));
#14483=CARTESIAN_POINT('',(1.65,18.,77.7));
#14484=CARTESIAN_POINT('',(1.65,18.,87.6));
#14485=CARTESIAN_POINT('Origin',(0.,18.,77.7));
#14486=CARTESIAN_POINT('Origin',(-32.,26.,115.8875));
#14487=CARTESIAN_POINT('',(-32.,25.,118.3875));
#14488=CARTESIAN_POINT('Origin',(-32.,25.,115.8875));
#14489=CARTESIAN_POINT('',(-32.,10.,118.3875));
#14490=CARTESIAN_POINT('',(-32.,26.,118.3875));
#14491=CARTESIAN_POINT('Origin',(-32.,10.,115.8875));
#14492=CARTESIAN_POINT('Origin',(32.,26.,115.8875));
#14493=CARTESIAN_POINT('',(32.,25.,118.3875));
#14494=CARTESIAN_POINT('Origin',(32.,25.,115.8875));
#14495=CARTESIAN_POINT('',(32.,10.,118.3875));
#14496=CARTESIAN_POINT('',(32.,26.,118.3875));
#14497=CARTESIAN_POINT('Origin',(32.,10.,115.8875));
#14498=CARTESIAN_POINT('Origin',(0.,17.,113.));
#14499=CARTESIAN_POINT('',(-7.53157781475623E-16,17.,119.15));
#14500=CARTESIAN_POINT('Origin',(0.,17.,113.));
#14501=CARTESIAN_POINT('',(-7.53157781475623E-16,-2.,119.15));
#14502=CARTESIAN_POINT('',(-7.53157781475623E-16,17.,119.15));
#14503=CARTESIAN_POINT('Origin',(0.,-2.,113.));
#14504=CARTESIAN_POINT('Origin',(-50.8,25.,82.2));
#14505=CARTESIAN_POINT('',(7.7,25.,82.2));
#14506=CARTESIAN_POINT('',(7.7,-2.,82.2));
#14507=CARTESIAN_POINT('',(7.7,25.,82.2));
#14508=CARTESIAN_POINT('',(50.8,25.,82.2));
#14509=CARTESIAN_POINT('',(-50.8,25.,82.2));
#14510=CARTESIAN_POINT('',(50.8,-2.,82.2));
#14511=CARTESIAN_POINT('',(50.8,25.,82.2));
#14512=CARTESIAN_POINT('',(-50.8,-2.,82.2));
#14513=CARTESIAN_POINT('Origin',(-50.8,25.,82.2));
#14514=CARTESIAN_POINT('',(-7.7,-2.,82.2));
#14515=CARTESIAN_POINT('',(-7.7,25.,82.2));
#14516=CARTESIAN_POINT('',(-7.7,25.,82.2));
#14517=CARTESIAN_POINT('',(-50.8,-2.,82.2));
#14518=CARTESIAN_POINT('',(-50.8,-2.,82.2));
#14519=CARTESIAN_POINT('',(-50.8,25.,82.2));
#14520=CARTESIAN_POINT('',(-50.8,25.,82.2));
#14521=CARTESIAN_POINT('',(-50.8,25.,82.2));
#14522=CARTESIAN_POINT('Origin',(-50.8,25.,127.35));
#14523=CARTESIAN_POINT('',(-50.8,-2.,127.35));
#14524=CARTESIAN_POINT('',(-50.8,-2.,127.35));
#14525=CARTESIAN_POINT('',(-50.8,25.,127.35));
#14526=CARTESIAN_POINT('',(-50.8,25.,127.35));
#14527=CARTESIAN_POINT('',(-50.8,25.,127.35));
#14528=CARTESIAN_POINT('Origin',(-44.8,25.,133.35));
#14529=CARTESIAN_POINT('',(-44.8,-2.,133.35));
#14530=CARTESIAN_POINT('',(-44.8,-2.,133.35));
#14531=CARTESIAN_POINT('',(-44.8,25.,133.35));
#14532=CARTESIAN_POINT('',(-44.8,25.,133.35));
#14533=CARTESIAN_POINT('',(-44.8,25.,133.35));
#14534=CARTESIAN_POINT('Origin',(44.8000000000001,25.,133.35));
#14535=CARTESIAN_POINT('',(44.8000000000001,-2.,133.35));
#14536=CARTESIAN_POINT('',(44.8000000000001,-2.,133.35));
#14537=CARTESIAN_POINT('',(44.8000000000001,25.,133.35));
#14538=CARTESIAN_POINT('',(44.8000000000001,25.,133.35));
#14539=CARTESIAN_POINT('',(44.8000000000001,25.,133.35));
#14540=CARTESIAN_POINT('Origin',(50.8,25.,127.35));
#14541=CARTESIAN_POINT('',(50.8,-2.,127.35));
#14542=CARTESIAN_POINT('',(50.8,-2.,127.35));
#14543=CARTESIAN_POINT('',(50.8,25.,127.35));
#14544=CARTESIAN_POINT('',(50.8,25.,127.35));
#14545=CARTESIAN_POINT('',(50.8,25.,127.35));
#14546=CARTESIAN_POINT('Origin',(50.8,25.,82.2));
#14547=CARTESIAN_POINT('',(50.8,-2.,82.2));
#14548=CARTESIAN_POINT('',(50.8,25.,82.2));
#14549=CARTESIAN_POINT('Origin',(0.,25.,0.));
#14550=CARTESIAN_POINT('',(7.7,25.,77.7));
#14551=CARTESIAN_POINT('',(7.7,25.,84.2));
#14552=CARTESIAN_POINT('',(-7.7,25.,77.7));
#14553=CARTESIAN_POINT('',(-7.7,25.,77.7));
#14554=CARTESIAN_POINT('',(-7.7,25.,84.2));
#14555=CARTESIAN_POINT('Origin',(0.,-2.,0.));
#14556=CARTESIAN_POINT('',(-7.7,-2.,77.7));
#14557=CARTESIAN_POINT('',(-7.7,-2.,84.2));
#14558=CARTESIAN_POINT('',(7.7,-2.,77.7));
#14559=CARTESIAN_POINT('',(-7.7,-2.,77.7));
#14560=CARTESIAN_POINT('',(7.7,-2.,84.2));
#14561=CARTESIAN_POINT('Origin',(7.7,-2.,84.2));
#14562=CARTESIAN_POINT('',(7.7,-2.,77.7));
#14563=CARTESIAN_POINT('Origin',(-7.7,-2.,84.2));
#14564=CARTESIAN_POINT('',(-7.7,-2.,77.7));
#14565=CARTESIAN_POINT('Origin',(0.,0.,77.7));
#14566=CARTESIAN_POINT('Origin',(0.,17.,113.));
#14567=CARTESIAN_POINT('Origin',(32.,10.,115.8875));
#14568=CARTESIAN_POINT('Origin',(-32.,10.,115.8875));
#14569=CARTESIAN_POINT('Origin',(0.,18.,87.6));
#14570=CARTESIAN_POINT('Origin',(0.,5.,87.6));
#14571=CARTESIAN_POINT('',(0.,0.,0.));
#14572=CARTESIAN_POINT('Origin',(68.,45.2333,33.9));
#14573=CARTESIAN_POINT('',(-68.,45.2333,33.9));
#14574=CARTESIAN_POINT('',(-68.,33.7,16.6));
#14575=CARTESIAN_POINT('',(-68.,45.2333,33.9));
#14576=CARTESIAN_POINT('',(68.,33.7,16.6));
#14577=CARTESIAN_POINT('',(68.,33.7,16.6));
#14578=CARTESIAN_POINT('',(68.,45.2333,33.9));
#14579=CARTESIAN_POINT('',(68.,45.2333,33.9));
#14580=CARTESIAN_POINT('',(68.,45.2333,33.9));
#14581=CARTESIAN_POINT('Origin',(68.,33.7,16.6));
#14582=CARTESIAN_POINT('',(-68.,36.4,16.6));
#14583=CARTESIAN_POINT('',(-68.,33.7,16.6));
#14584=CARTESIAN_POINT('',(68.,36.4,16.6));
#14585=CARTESIAN_POINT('',(68.,36.4,16.6));
#14586=CARTESIAN_POINT('',(68.,33.7,16.6));
#14587=CARTESIAN_POINT('Origin',(68.,36.4,16.6));
#14588=CARTESIAN_POINT('',(-68.,47.9333,33.9));
#14589=CARTESIAN_POINT('',(-68.,36.4,16.6));
#14590=CARTESIAN_POINT('',(68.,47.9333,33.9));
#14591=CARTESIAN_POINT('',(68.,47.9333,33.9));
#14592=CARTESIAN_POINT('',(68.,36.4,16.6));
#14593=CARTESIAN_POINT('Origin',(68.,47.9333,33.9));
#14594=CARTESIAN_POINT('',(-68.,47.9333,33.9));
#14595=CARTESIAN_POINT('',(68.,47.9333,33.9));
#14596=CARTESIAN_POINT('Origin',(68.,0.,0.));
#14597=CARTESIAN_POINT('Origin',(-68.,0.,0.));
#14598=CARTESIAN_POINT('',(0.,0.,0.));
#14599=CARTESIAN_POINT('Origin',(45.2333,49.,67.9));
#14600=CARTESIAN_POINT('',(33.7,-49.,50.6));
#14601=CARTESIAN_POINT('',(45.2333,-49.,67.9));
#14602=CARTESIAN_POINT('',(45.2333,-49.,67.9));
#14603=CARTESIAN_POINT('',(45.2333,49.,67.9));
#14604=CARTESIAN_POINT('',(45.2333,49.,67.9));
#14605=CARTESIAN_POINT('',(33.7,49.,50.6));
#14606=CARTESIAN_POINT('',(45.2333,49.,67.9));
#14607=CARTESIAN_POINT('',(33.7,49.,50.6));
#14608=CARTESIAN_POINT('Origin',(47.9333,49.,67.9));
#14609=CARTESIAN_POINT('',(47.9333,-49.,67.9));
#14610=CARTESIAN_POINT('',(47.9333,-49.,67.9));
#14611=CARTESIAN_POINT('',(47.9333,49.,67.9));
#14612=CARTESIAN_POINT('',(47.9333,49.,67.9));
#14613=CARTESIAN_POINT('',(47.9333,49.,67.9));
#14614=CARTESIAN_POINT('Origin',(36.4,49.,50.6));
#14615=CARTESIAN_POINT('',(36.4,-49.,50.6));
#14616=CARTESIAN_POINT('',(36.4,-49.,50.6));
#14617=CARTESIAN_POINT('',(36.4,49.,50.6));
#14618=CARTESIAN_POINT('',(36.4,49.,50.6));
#14619=CARTESIAN_POINT('',(36.4,49.,50.6));
#14620=CARTESIAN_POINT('Origin',(33.7,49.,50.6));
#14621=CARTESIAN_POINT('',(33.7,-49.,50.6));
#14622=CARTESIAN_POINT('',(33.7,49.,50.6));
#14623=CARTESIAN_POINT('Origin',(0.,49.,0.));
#14624=CARTESIAN_POINT('Origin',(0.,-49.,0.));
#14625=CARTESIAN_POINT('',(0.,0.,0.));
#14626=CARTESIAN_POINT('Origin',(0.,18.,74.3));
#14627=CARTESIAN_POINT('',(3.7,18.,74.3));
#14628=CARTESIAN_POINT('Origin',(0.,18.,74.3));
#14629=CARTESIAN_POINT('',(3.7,18.,72.3));
#14630=CARTESIAN_POINT('',(3.7,18.,74.3));
#14631=CARTESIAN_POINT('Origin',(0.,18.,72.3));
#14632=CARTESIAN_POINT('Origin',(0.,5.,74.3));
#14633=CARTESIAN_POINT('',(3.7,5.,74.3));
#14634=CARTESIAN_POINT('Origin',(0.,5.,74.3));
#14635=CARTESIAN_POINT('',(3.7,5.,72.3));
#14636=CARTESIAN_POINT('',(3.7,5.,74.3));
#14637=CARTESIAN_POINT('Origin',(0.,5.,72.3));
#14638=CARTESIAN_POINT('Origin',(0.,5.,78.5));
#14639=CARTESIAN_POINT('',(2.2,5.,77.7));
#14640=CARTESIAN_POINT('Origin',(0.,5.,77.7));
#14641=CARTESIAN_POINT('',(2.2,5.,74.3));
#14642=CARTESIAN_POINT('',(2.2,5.,78.5));
#14643=CARTESIAN_POINT('Origin',(0.,5.,74.3));
#14644=CARTESIAN_POINT('Origin',(0.,18.,78.5));
#14645=CARTESIAN_POINT('',(2.2,18.,77.7));
#14646=CARTESIAN_POINT('Origin',(0.,18.,77.7));
#14647=CARTESIAN_POINT('',(2.2,18.,74.3));
#14648=CARTESIAN_POINT('',(2.2,18.,78.5));
#14649=CARTESIAN_POINT('Origin',(0.,18.,74.3));
#14650=CARTESIAN_POINT('Origin',(15.7,-2.,77.7));
#14651=CARTESIAN_POINT('',(15.7,-2.,72.3));
#14652=CARTESIAN_POINT('',(15.7,25.,72.3));
#14653=CARTESIAN_POINT('',(15.7,-2.,72.3));
#14654=CARTESIAN_POINT('',(15.7,25.,77.7));
#14655=CARTESIAN_POINT('',(15.7,25.,77.7));
#14656=CARTESIAN_POINT('',(15.7,-2.,77.7));
#14657=CARTESIAN_POINT('',(15.7,-2.,77.7));
#14658=CARTESIAN_POINT('',(15.7,-2.,77.7));
#14659=CARTESIAN_POINT('Origin',(-15.7,25.,77.7));
#14660=CARTESIAN_POINT('',(-15.7,25.,72.3));
#14661=CARTESIAN_POINT('',(-15.7,25.,72.3));
#14662=CARTESIAN_POINT('',(-15.7,25.,77.7));
#14663=CARTESIAN_POINT('',(-15.7,25.,77.7));
#14664=CARTESIAN_POINT('',(-15.7,25.,77.7));
#14665=CARTESIAN_POINT('Origin',(-15.7,-2.,77.7));
#14666=CARTESIAN_POINT('',(-15.7,-2.,72.3));
#14667=CARTESIAN_POINT('',(-15.7,-2.,72.3));
#14668=CARTESIAN_POINT('',(-15.7,-2.,77.7));
#14669=CARTESIAN_POINT('',(-15.7,-2.,77.7));
#14670=CARTESIAN_POINT('',(-15.7,-2.,77.7));
#14671=CARTESIAN_POINT('Origin',(-15.7,-2.,77.7));
#14672=CARTESIAN_POINT('',(-15.7,-2.,72.3));
#14673=CARTESIAN_POINT('',(-15.7,-2.,77.7));
#14674=CARTESIAN_POINT('Origin',(0.,0.,77.7));
#14675=CARTESIAN_POINT('Origin',(0.,0.,72.3));
#14676=CARTESIAN_POINT('Origin',(0.,5.,74.3));
#14677=CARTESIAN_POINT('Origin',(0.,18.,74.3));
#14678=CARTESIAN_POINT('',(0.,0.,0.));
#14679=CARTESIAN_POINT('Origin',(0.,0.,-5.));
#14680=CARTESIAN_POINT('',(5.55,-6.79678973526781E-16,46.));
#14681=CARTESIAN_POINT('Origin',(0.,0.,46.));
#14682=CARTESIAN_POINT('',(5.55,-6.79678973526781E-16,260.));
#14683=CARTESIAN_POINT('',(5.55,-6.79678973526781E-16,-5.));
#14684=CARTESIAN_POINT('Origin',(0.,0.,260.));
#14685=CARTESIAN_POINT('Origin',(0.,0.,-5.));
#14686=CARTESIAN_POINT('',(6.,-7.34788079488412E-16,40.));
#14687=CARTESIAN_POINT('Origin',(0.,0.,40.));
#14688=CARTESIAN_POINT('',(6.,-7.34788079488412E-16,46.));
#14689=CARTESIAN_POINT('',(6.,-7.34788079488412E-16,-5.));
#14690=CARTESIAN_POINT('Origin',(0.,0.,46.));
#14691=CARTESIAN_POINT('Origin',(0.,0.,-5.));
#14692=CARTESIAN_POINT('',(9.,-1.10218211923262E-15,36.));
#14693=CARTESIAN_POINT('Origin',(0.,0.,36.));
#14694=CARTESIAN_POINT('',(9.,-1.10218211923262E-15,40.));
#14695=CARTESIAN_POINT('',(9.,-1.10218211923262E-15,-5.));
#14696=CARTESIAN_POINT('Origin',(0.,0.,40.));
#14697=CARTESIAN_POINT('Origin',(0.,0.,-5.));
#14698=CARTESIAN_POINT('',(6.,-7.34788079488412E-16,14.));
#14699=CARTESIAN_POINT('Origin',(0.,0.,14.));
#14700=CARTESIAN_POINT('',(6.,-7.34788079488412E-16,36.));
#14701=CARTESIAN_POINT('',(6.,-7.34788079488412E-16,-5.));
#14702=CARTESIAN_POINT('Origin',(0.,0.,36.));
#14703=CARTESIAN_POINT('Origin',(0.,0.,-5.));
#14704=CARTESIAN_POINT('',(4.,-4.89858719658941E-16,0.));
#14705=CARTESIAN_POINT('Origin',(0.,0.,0.));
#14706=CARTESIAN_POINT('',(4.,-4.89858719658941E-16,14.));
#14707=CARTESIAN_POINT('',(4.,-4.89858719658941E-16,-5.));
#14708=CARTESIAN_POINT('Origin',(0.,0.,14.));
#14709=CARTESIAN_POINT('Origin',(0.,0.,0.));
#14710=CARTESIAN_POINT('Origin',(4.,0.,14.));
#14711=CARTESIAN_POINT('Origin',(6.,0.,36.));
#14712=CARTESIAN_POINT('Origin',(9.,0.,40.));
#14713=CARTESIAN_POINT('Origin',(6.,0.,46.));
#14714=CARTESIAN_POINT('Origin',(5.55,0.,260.));
#14715=CARTESIAN_POINT('',(0.,0.,0.));
#14716=CARTESIAN_POINT('Origin',(0.,0.,-5.));
#14717=CARTESIAN_POINT('',(7.15,-8.75622461390358E-16,46.));
#14718=CARTESIAN_POINT('Origin',(0.,0.,46.));
#14719=CARTESIAN_POINT('',(7.15,-8.75622461390358E-16,230.));
#14720=CARTESIAN_POINT('',(7.15,-8.75622461390358E-16,-5.));
#14721=CARTESIAN_POINT('Origin',(0.,0.,230.));
#14722=CARTESIAN_POINT('Origin',(0.,0.,-5.));
#14723=CARTESIAN_POINT('',(6.,-7.34788079488412E-16,40.));
#14724=CARTESIAN_POINT('Origin',(0.,0.,40.));
#14725=CARTESIAN_POINT('',(6.,-7.34788079488412E-16,46.));
#14726=CARTESIAN_POINT('',(6.,-7.34788079488412E-16,-5.));
#14727=CARTESIAN_POINT('Origin',(0.,0.,46.));
#14728=CARTESIAN_POINT('Origin',(0.,0.,-5.));
#14729=CARTESIAN_POINT('',(9.,-1.10218211923262E-15,36.));
#14730=CARTESIAN_POINT('Origin',(0.,0.,36.));
#14731=CARTESIAN_POINT('',(9.,-1.10218211923262E-15,40.));
#14732=CARTESIAN_POINT('',(9.,-1.10218211923262E-15,-5.));
#14733=CARTESIAN_POINT('Origin',(0.,0.,40.));
#14734=CARTESIAN_POINT('Origin',(0.,0.,-5.));
#14735=CARTESIAN_POINT('',(6.,-7.34788079488412E-16,14.));
#14736=CARTESIAN_POINT('Origin',(0.,0.,14.));
#14737=CARTESIAN_POINT('',(6.,-7.34788079488412E-16,36.));
#14738=CARTESIAN_POINT('',(6.,-7.34788079488412E-16,-5.));
#14739=CARTESIAN_POINT('Origin',(0.,0.,36.));
#14740=CARTESIAN_POINT('Origin',(0.,0.,-5.));
#14741=CARTESIAN_POINT('',(4.,-4.89858719658941E-16,0.));
#14742=CARTESIAN_POINT('Origin',(0.,0.,0.));
#14743=CARTESIAN_POINT('',(4.,-4.89858719658941E-16,14.));
#14744=CARTESIAN_POINT('',(4.,-4.89858719658941E-16,-5.));
#14745=CARTESIAN_POINT('Origin',(0.,0.,14.));
#14746=CARTESIAN_POINT('Origin',(0.,0.,0.));
#14747=CARTESIAN_POINT('Origin',(4.,0.,14.));
#14748=CARTESIAN_POINT('Origin',(6.,0.,36.));
#14749=CARTESIAN_POINT('Origin',(9.,0.,40.));
#14750=CARTESIAN_POINT('Origin',(6.,0.,46.));
#14751=CARTESIAN_POINT('Origin',(7.15,0.,230.));
#14752=CARTESIAN_POINT('',(0.,0.,0.));
#14753=CARTESIAN_POINT('Origin',(12.,0.,11.));
#14754=CARTESIAN_POINT('',(-3.2,-2.69422295812418E-16,8.8));
#14755=CARTESIAN_POINT('Origin',(-3.2,0.,11.));
#14756=CARTESIAN_POINT('',(-10.,-2.69422295812418E-16,8.8));
#14757=CARTESIAN_POINT('',(12.,-2.69422295812418E-16,8.8));
#14758=CARTESIAN_POINT('',(-10.,4.3528800643699E-16,13.2));
#14759=CARTESIAN_POINT('Ctrl Pts',(-10.,-2.77555756156289E-16,8.8));
#14760=CARTESIAN_POINT('Ctrl Pts',(-10.,-0.277203807947464,8.8));
#14761=CARTESIAN_POINT('Ctrl Pts',(-9.98731242652721,-0.572272533644394,
8.85558441201917));
#14762=CARTESIAN_POINT('Ctrl Pts',(-9.94146891308711,-1.1140472218706,9.08038732993933));
#14763=CARTESIAN_POINT('Ctrl Pts',(-9.90893754512743,-1.36082632626377,
9.24955648904296));
#14764=CARTESIAN_POINT('Ctrl Pts',(-9.84757782914463,-1.75045962433893,
9.63918978711812));
#14765=CARTESIAN_POINT('Ctrl Pts',(-9.81469565126959,-1.91961618195498,
9.88596209803831));
#14766=CARTESIAN_POINT('Ctrl Pts',(-9.76804398559235,-2.14440993937815,
10.4277129969916));
#14767=CARTESIAN_POINT('Ctrl Pts',(-9.75499871860576,-2.2,10.7227732634396));
#14768=CARTESIAN_POINT('Ctrl Pts',(-9.75499871860576,-2.2,11.2772267365604));
#14769=CARTESIAN_POINT('Ctrl Pts',(-9.76804398559235,-2.14440993937815,
11.5722870030084));
#14770=CARTESIAN_POINT('Ctrl Pts',(-9.81469565126959,-1.91961618195498,
12.1140379019617));
#14771=CARTESIAN_POINT('Ctrl Pts',(-9.84757782914463,-1.75045962433893,
12.3608102128819));
#14772=CARTESIAN_POINT('Ctrl Pts',(-9.90893754512743,-1.36082632626377,
12.750443510957));
#14773=CARTESIAN_POINT('Ctrl Pts',(-9.94146891308711,-1.1140472218706,12.9196126700607));
#14774=CARTESIAN_POINT('Ctrl Pts',(-9.98731242652721,-0.572272533644395,
13.1444155879808));
#14775=CARTESIAN_POINT('Ctrl Pts',(-10.,-0.277203807947464,13.2));
#14776=CARTESIAN_POINT('Ctrl Pts',(-10.,-2.08166817117217E-16,13.2));
#14777=CARTESIAN_POINT('Ctrl Pts',(-10.,-2.08166817117217E-16,13.2));
#14778=CARTESIAN_POINT('Ctrl Pts',(-10.,0.277203807947464,13.2));
#14779=CARTESIAN_POINT('Ctrl Pts',(-9.98731242652721,0.572272533644394,
13.1444155879808));
#14780=CARTESIAN_POINT('Ctrl Pts',(-9.94146891308711,1.1140472218706,12.9196126700607));
#14781=CARTESIAN_POINT('Ctrl Pts',(-9.90893754512743,1.36082632626377,12.750443510957));
#14782=CARTESIAN_POINT('Ctrl Pts',(-9.84757782914463,1.75045962433893,12.3608102128819));
#14783=CARTESIAN_POINT('Ctrl Pts',(-9.81469565126959,1.91961618195498,12.1140379019617));
#14784=CARTESIAN_POINT('Ctrl Pts',(-9.76804398559235,2.14440993937815,11.5722870030084));
#14785=CARTESIAN_POINT('Ctrl Pts',(-9.75499871860576,2.2,11.2772267365604));
#14786=CARTESIAN_POINT('Ctrl Pts',(-9.75499871860576,2.2,11.));
#14787=CARTESIAN_POINT('Ctrl Pts',(-9.75499871860576,2.2,10.7227732634396));
#14788=CARTESIAN_POINT('Ctrl Pts',(-9.76804398559235,2.14440993937815,10.4277129969916));
#14789=CARTESIAN_POINT('Ctrl Pts',(-9.81469565126959,1.91961618195498,9.88596209803831));
#14790=CARTESIAN_POINT('Ctrl Pts',(-9.84757782914463,1.75045962433893,9.63918978711812));
#14791=CARTESIAN_POINT('Ctrl Pts',(-9.90893754512743,1.36082632626377,9.24955648904296));
#14792=CARTESIAN_POINT('Ctrl Pts',(-9.94146891308711,1.1140472218706,9.08038732993933));
#14793=CARTESIAN_POINT('Ctrl Pts',(-9.98731242652721,0.572272533644394,
8.85558441201917));
#14794=CARTESIAN_POINT('Ctrl Pts',(-10.,0.277203807947463,8.8));
#14795=CARTESIAN_POINT('Ctrl Pts',(-10.,-4.16333634234434E-16,8.8));
#14796=CARTESIAN_POINT('Origin',(12.,0.,11.));
#14797=CARTESIAN_POINT('',(10.,-4.3528800643699E-16,13.2));
#14798=CARTESIAN_POINT('',(10.,-2.69422295812418E-16,8.8));
#14799=CARTESIAN_POINT('Ctrl Pts',(10.,-5.55111512312578E-16,13.2));
#14800=CARTESIAN_POINT('Ctrl Pts',(10.,-0.277203807947464,13.2));
#14801=CARTESIAN_POINT('Ctrl Pts',(9.98731242652721,-0.572272533644394,
13.1444155879808));
#14802=CARTESIAN_POINT('Ctrl Pts',(9.94146891308711,-1.1140472218706,12.9196126700607));
#14803=CARTESIAN_POINT('Ctrl Pts',(9.90893754512743,-1.36082632626377,12.750443510957));
#14804=CARTESIAN_POINT('Ctrl Pts',(9.84757782914463,-1.75045962433893,12.3608102128819));
#14805=CARTESIAN_POINT('Ctrl Pts',(9.81469565126959,-1.91961618195498,12.1140379019617));
#14806=CARTESIAN_POINT('Ctrl Pts',(9.76804398559235,-2.14440993937815,11.5722870030084));
#14807=CARTESIAN_POINT('Ctrl Pts',(9.75499871860576,-2.2,11.2772267365605));
#14808=CARTESIAN_POINT('Ctrl Pts',(9.75499871860576,-2.2,10.7227732634396));
#14809=CARTESIAN_POINT('Ctrl Pts',(9.76804398559235,-2.14440993937815,10.4277129969916));
#14810=CARTESIAN_POINT('Ctrl Pts',(9.81469565126959,-1.91961618195498,9.88596209803831));
#14811=CARTESIAN_POINT('Ctrl Pts',(9.84757782914463,-1.75045962433893,9.63918978711812));
#14812=CARTESIAN_POINT('Ctrl Pts',(9.90893754512743,-1.36082632626377,9.24955648904296));
#14813=CARTESIAN_POINT('Ctrl Pts',(9.94146891308711,-1.1140472218706,9.08038732993933));
#14814=CARTESIAN_POINT('Ctrl Pts',(9.98731242652721,-0.572272533644394,
8.85558441201917));
#14815=CARTESIAN_POINT('Ctrl Pts',(10.,-0.277203807947463,8.8));
#14816=CARTESIAN_POINT('Ctrl Pts',(10.,4.16333634234434E-16,8.8));
#14817=CARTESIAN_POINT('',(3.2,-2.69422295812418E-16,8.8));
#14818=CARTESIAN_POINT('',(12.,-2.69422295812418E-16,8.8));
#14819=CARTESIAN_POINT('Origin',(3.2,0.,11.));
#14820=CARTESIAN_POINT('Ctrl Pts',(10.,1.38777878078145E-16,8.8));
#14821=CARTESIAN_POINT('Ctrl Pts',(10.,0.277203807947464,8.8));
#14822=CARTESIAN_POINT('Ctrl Pts',(9.98731242652721,0.572272533644394,8.85558441201917));
#14823=CARTESIAN_POINT('Ctrl Pts',(9.94146891308711,1.1140472218706,9.08038732993933));
#14824=CARTESIAN_POINT('Ctrl Pts',(9.90893754512743,1.36082632626377,9.24955648904296));
#14825=CARTESIAN_POINT('Ctrl Pts',(9.84757782914463,1.75045962433893,9.63918978711812));
#14826=CARTESIAN_POINT('Ctrl Pts',(9.81469565126959,1.91961618195498,9.88596209803831));
#14827=CARTESIAN_POINT('Ctrl Pts',(9.76804398559235,2.14440993937815,10.4277129969916));
#14828=CARTESIAN_POINT('Ctrl Pts',(9.75499871860576,2.2,10.7227732634396));
#14829=CARTESIAN_POINT('Ctrl Pts',(9.75499871860576,2.2,11.));
#14830=CARTESIAN_POINT('Ctrl Pts',(9.75499871860576,2.2,11.2772267365604));
#14831=CARTESIAN_POINT('Ctrl Pts',(9.76804398559235,2.14440993937815,11.5722870030084));
#14832=CARTESIAN_POINT('Ctrl Pts',(9.81469565126959,1.91961618195498,12.1140379019617));
#14833=CARTESIAN_POINT('Ctrl Pts',(9.84757782914463,1.75045962433893,12.3608102128819));
#14834=CARTESIAN_POINT('Ctrl Pts',(9.90893754512743,1.36082632626377,12.750443510957));
#14835=CARTESIAN_POINT('Ctrl Pts',(9.94146891308711,1.1140472218706,12.9196126700607));
#14836=CARTESIAN_POINT('Ctrl Pts',(9.98731242652721,0.572272533644393,13.1444155879808));
#14837=CARTESIAN_POINT('Ctrl Pts',(10.,0.277203807947463,13.2));
#14838=CARTESIAN_POINT('Ctrl Pts',(10.,-6.24500451351651E-16,13.2));
#14839=CARTESIAN_POINT('Origin',(0.,0.,-5.));
#14840=CARTESIAN_POINT('',(6.,-7.34788079488412E-16,172.));
#14841=CARTESIAN_POINT('Origin',(0.,0.,172.));
#14842=CARTESIAN_POINT('',(6.,-7.34788079488412E-16,190.));
#14843=CARTESIAN_POINT('',(6.,-7.34788079488412E-16,-5.));
#14844=CARTESIAN_POINT('Origin',(0.,0.,190.));
#14845=CARTESIAN_POINT('Origin',(0.,0.,-5.));
#14846=CARTESIAN_POINT('',(8.75,-1.07156594925393E-15,23.));
#14847=CARTESIAN_POINT('Origin',(0.,0.,23.));
#14848=CARTESIAN_POINT('',(8.75,-1.07156594925393E-15,172.));
#14849=CARTESIAN_POINT('',(8.75,-1.07156594925393E-15,-5.));
#14850=CARTESIAN_POINT('Origin',(0.,0.,172.));
#14851=CARTESIAN_POINT('Origin',(0.,0.,-5.));
#14852=CARTESIAN_POINT('',(-3.2,-9.47417542586161,0.));
#14853=CARTESIAN_POINT('',(-3.2,9.47417542586161,0.));
#14854=CARTESIAN_POINT('Origin',(0.,0.,0.));
#14855=CARTESIAN_POINT('',(-3.2,-9.47417542586161,20.));
#14856=CARTESIAN_POINT('',(-3.2,-9.47417542586161,-5.));
#14857=CARTESIAN_POINT('',(3.2,-9.47417542586161,20.));
#14858=CARTESIAN_POINT('Origin',(0.,0.,20.));
#14859=CARTESIAN_POINT('',(3.2,-9.47417542586161,0.));
#14860=CARTESIAN_POINT('',(3.2,-9.47417542586161,-5.));
#14861=CARTESIAN_POINT('',(10.,-1.22464679914735E-15,0.));
#14862=CARTESIAN_POINT('Origin',(0.,0.,0.));
#14863=CARTESIAN_POINT('',(10.,-1.22464679914735E-15,-5.));
#14864=CARTESIAN_POINT('',(10.,-1.22464679914735E-15,23.));
#14865=CARTESIAN_POINT('',(10.,-1.22464679914735E-15,-5.));
#14866=CARTESIAN_POINT('Origin',(0.,0.,23.));
#14867=CARTESIAN_POINT('',(3.2,9.47417542586161,0.));
#14868=CARTESIAN_POINT('Origin',(0.,0.,0.));
#14869=CARTESIAN_POINT('',(3.2,9.47417542586161,20.));
#14870=CARTESIAN_POINT('',(3.2,9.47417542586161,-5.));
#14871=CARTESIAN_POINT('',(-3.2,9.47417542586161,20.));
#14872=CARTESIAN_POINT('Origin',(0.,0.,20.));
#14873=CARTESIAN_POINT('',(-3.2,9.47417542586161,-5.));
#14874=CARTESIAN_POINT('Origin',(0.,0.,0.));
#14875=CARTESIAN_POINT('',(-3.2,0.,0.));
#14876=CARTESIAN_POINT('Origin',(0.,0.,0.));
#14877=CARTESIAN_POINT('',(3.2,0.,0.));
#14878=CARTESIAN_POINT('Origin',(10.,0.,23.));
#14879=CARTESIAN_POINT('Origin',(8.75,0.,172.));
#14880=CARTESIAN_POINT('Origin',(6.,0.,190.));
#14881=CARTESIAN_POINT('Origin',(-3.2,11.,20.));
#14882=CARTESIAN_POINT('',(-3.2,11.,20.));
#14883=CARTESIAN_POINT('Origin',(3.2,-11.,20.));
#14884=CARTESIAN_POINT('',(3.2,-11.,20.));
#14885=CARTESIAN_POINT('Origin',(0.,0.,20.));
#14886=CARTESIAN_POINT('',(0.,0.,0.));
#14887=CARTESIAN_POINT('Origin',(12.,0.,21.));
#14888=CARTESIAN_POINT('',(12.,-7.04171909509728E-16,15.25));
#14889=CARTESIAN_POINT('Origin',(12.,0.,21.));
#14890=CARTESIAN_POINT('',(-12.,-7.04171909509728E-16,15.25));
#14891=CARTESIAN_POINT('',(12.,-7.04171909509728E-16,15.25));
#14892=CARTESIAN_POINT('Origin',(-12.,0.,21.));
#14893=CARTESIAN_POINT('Origin',(12.,0.,0.));
#14894=CARTESIAN_POINT('',(12.,11.,34.3));
#14895=CARTESIAN_POINT('',(12.,-11.,34.3));
#14896=CARTESIAN_POINT('',(12.,-11.,34.3));
#14897=CARTESIAN_POINT('',(12.,-11.,10.3));
#14898=CARTESIAN_POINT('',(12.,-11.,10.3));
#14899=CARTESIAN_POINT('',(12.,11.,10.3));
#14900=CARTESIAN_POINT('',(12.,-11.,10.3));
#14901=CARTESIAN_POINT('',(12.,11.,10.3));
#14902=CARTESIAN_POINT('Origin',(-12.,0.,0.));
#14903=CARTESIAN_POINT('',(-12.,11.,34.3));
#14904=CARTESIAN_POINT('',(-12.,-11.,34.3));
#14905=CARTESIAN_POINT('',(-12.,-11.,34.3));
#14906=CARTESIAN_POINT('',(-12.,11.,10.3));
#14907=CARTESIAN_POINT('',(-12.,11.,10.3));
#14908=CARTESIAN_POINT('',(-12.,-11.,10.3));
#14909=CARTESIAN_POINT('',(-12.,-11.,10.3));
#14910=CARTESIAN_POINT('',(-12.,-11.,10.3));
#14911=CARTESIAN_POINT('Origin',(12.,-11.,34.3));
#14912=CARTESIAN_POINT('',(12.,-11.,34.3));
#14913=CARTESIAN_POINT('',(12.,11.,34.3));
#14914=CARTESIAN_POINT('Origin',(12.,-11.,10.3));
#14915=CARTESIAN_POINT('',(12.,-11.,10.3));
#14916=CARTESIAN_POINT('Origin',(12.,-11.,10.3));
#14917=CARTESIAN_POINT('',(12.,11.,10.3));
#14918=CARTESIAN_POINT('Origin',(12.,11.,10.3));
#14919=CARTESIAN_POINT('',(0.,0.,0.));
#14920=CARTESIAN_POINT('Origin',(0.,12.,55.));
#14921=CARTESIAN_POINT('',(-9.00115397373305E-16,12.,62.35));
#14922=CARTESIAN_POINT('Origin',(0.,12.,55.));
#14923=CARTESIAN_POINT('',(-9.00115397373305E-16,-12.,62.35));
#14924=CARTESIAN_POINT('',(-9.00115397373305E-16,12.,62.35));
#14925=CARTESIAN_POINT('Origin',(0.,-12.,55.));
#14926=CARTESIAN_POINT('Origin',(0.,12.,0.));
#14927=CARTESIAN_POINT('',(11.,12.,68.3));
#14928=CARTESIAN_POINT('',(11.,12.,44.3));
#14929=CARTESIAN_POINT('',(11.,12.,44.3));
#14930=CARTESIAN_POINT('',(-11.,12.,44.3));
#14931=CARTESIAN_POINT('',(-11.,12.,44.3));
#14932=CARTESIAN_POINT('',(-11.,12.,68.3));
#14933=CARTESIAN_POINT('',(-11.,12.,44.3));
#14934=CARTESIAN_POINT('',(-11.,12.,68.3));
#14935=CARTESIAN_POINT('Origin',(0.,-12.,0.));
#14936=CARTESIAN_POINT('',(11.,-12.,68.3));
#14937=CARTESIAN_POINT('',(11.,-12.,44.3));
#14938=CARTESIAN_POINT('',(11.,-12.,44.3));
#14939=CARTESIAN_POINT('',(-11.,-12.,68.3));
#14940=CARTESIAN_POINT('',(-11.,-12.,68.3));
#14941=CARTESIAN_POINT('',(-11.,-12.,44.3));
#14942=CARTESIAN_POINT('',(-11.,-12.,44.3));
#14943=CARTESIAN_POINT('',(-11.,-12.,44.3));
#14944=CARTESIAN_POINT('Origin',(11.,12.,44.3));
#14945=CARTESIAN_POINT('',(11.,12.,44.3));
#14946=CARTESIAN_POINT('',(11.,12.,68.3));
#14947=CARTESIAN_POINT('Origin',(-11.,12.,44.3));
#14948=CARTESIAN_POINT('',(-11.,12.,44.3));
#14949=CARTESIAN_POINT('Origin',(-11.,12.,44.3));
#14950=CARTESIAN_POINT('',(-11.,12.,68.3));
#14951=CARTESIAN_POINT('Origin',(-11.,12.,68.3));
#14952=CARTESIAN_POINT('',(0.,0.,0.));
#14953=CARTESIAN_POINT('Origin',(4.,0.,80.));
#14954=CARTESIAN_POINT('',(3.,-2.69422295812417E-16,77.8));
#14955=CARTESIAN_POINT('Origin',(3.,0.,80.));
#14956=CARTESIAN_POINT('',(-3.,-2.69422295812417E-16,77.8));
#14957=CARTESIAN_POINT('',(4.,-2.69422295812417E-16,77.8));
#14958=CARTESIAN_POINT('Origin',(-3.,0.,80.));
#14959=CARTESIAN_POINT('Origin',(3.,0.,80.));
#14960=CARTESIAN_POINT('',(3.,-6.21185679917027E-21,73.));
#14961=CARTESIAN_POINT('Origin',(3.,0.,80.));
#14962=CARTESIAN_POINT('',(-3.,0.,73.));
#14963=CARTESIAN_POINT('Ctrl Pts',(3.,4.5102810375397E-16,73.));
#14964=CARTESIAN_POINT('Ctrl Pts',(3.,0.381867569598129,73.));
#14965=CARTESIAN_POINT('Ctrl Pts',(2.92268305871952,0.785938626528129,73.0342116500025));
#14966=CARTESIAN_POINT('Ctrl Pts',(2.61493784812886,1.52377016291608,73.1576296998384));
#14967=CARTESIAN_POINT('Ctrl Pts',(2.38476353394969,1.8578771531696,73.2453932009422));
#14968=CARTESIAN_POINT('Ctrl Pts',(1.85751648085586,2.38512420626343,73.4130574284979));
#14969=CARTESIAN_POINT('Ctrl Pts',(1.52354231756781,2.61502716928633,73.5046430803547));
#14970=CARTESIAN_POINT('Ctrl Pts',(0.786243067181792,2.92256178949426,73.6370868756761));
#14971=CARTESIAN_POINT('Ctrl Pts',(0.382390373241929,3.,73.6754446796632));
#14972=CARTESIAN_POINT('Ctrl Pts',(-0.382390373241929,3.,73.6754446796632));
#14973=CARTESIAN_POINT('Ctrl Pts',(-0.786243067181794,2.92256178949426,
73.6370868756761));
#14974=CARTESIAN_POINT('Ctrl Pts',(-1.52354231756781,2.61502716928633,73.5046430803547));
#14975=CARTESIAN_POINT('Ctrl Pts',(-1.85751648085586,2.38512420626343,73.4130574284979));
#14976=CARTESIAN_POINT('Ctrl Pts',(-2.38476353394969,1.8578771531696,73.2453932009422));
#14977=CARTESIAN_POINT('Ctrl Pts',(-2.61493784812886,1.52377016291608,73.1576296998384));
#14978=CARTESIAN_POINT('Ctrl Pts',(-2.92268305871952,0.785938626528129,
73.0342116500025));
#14979=CARTESIAN_POINT('Ctrl Pts',(-3.,0.381867569598128,73.));
#14980=CARTESIAN_POINT('Ctrl Pts',(-3.,0.,73.));
#14981=CARTESIAN_POINT('Origin',(-3.,0.,80.));
#14982=CARTESIAN_POINT('Ctrl Pts',(-3.,6.59194920871187E-16,73.));
#14983=CARTESIAN_POINT('Ctrl Pts',(-3.,-0.381867569598127,73.));
#14984=CARTESIAN_POINT('Ctrl Pts',(-2.92268305871952,-0.785938626528129,
73.0342116500025));
#14985=CARTESIAN_POINT('Ctrl Pts',(-2.61493784812886,-1.52377016291608,
73.1576296998384));
#14986=CARTESIAN_POINT('Ctrl Pts',(-2.38476353394969,-1.8578771531696,73.2453932009422));
#14987=CARTESIAN_POINT('Ctrl Pts',(-1.85751648085586,-2.38512420626343,
73.4130574284979));
#14988=CARTESIAN_POINT('Ctrl Pts',(-1.52354231756781,-2.61502716928633,
73.5046430803547));
#14989=CARTESIAN_POINT('Ctrl Pts',(-0.786243067181791,-2.92256178949426,
73.6370868756761));
#14990=CARTESIAN_POINT('Ctrl Pts',(-0.382390373241929,-3.,73.6754446796632));
#14991=CARTESIAN_POINT('Ctrl Pts',(0.,-3.,73.6754446796632));
#14992=CARTESIAN_POINT('Ctrl Pts',(0.382390373241929,-3.,73.6754446796632));
#14993=CARTESIAN_POINT('Ctrl Pts',(0.786243067181791,-2.92256178949426,
73.6370868756761));
#14994=CARTESIAN_POINT('Ctrl Pts',(1.52354231756781,-2.61502716928633,73.5046430803547));
#14995=CARTESIAN_POINT('Ctrl Pts',(1.85751648085586,-2.38512420626343,73.4130574284979));
#14996=CARTESIAN_POINT('Ctrl Pts',(2.38476353394969,-1.8578771531696,73.2453932009422));
#14997=CARTESIAN_POINT('Ctrl Pts',(2.61493784812886,-1.52377016291608,73.1576296998384));
#14998=CARTESIAN_POINT('Ctrl Pts',(2.92268305871952,-0.785938626528129,
73.0342116500025));
#14999=CARTESIAN_POINT('Ctrl Pts',(3.,-0.381867569598129,73.));
#15000=CARTESIAN_POINT('Ctrl Pts',(3.,-4.85722573273506E-16,73.));
#15001=CARTESIAN_POINT('Origin',(0.,0.,60.));
#15002=CARTESIAN_POINT('',(5.,-6.12323399573677E-16,0.));
#15003=CARTESIAN_POINT('Origin',(0.,0.,0.));
#15004=CARTESIAN_POINT('',(5.,-6.12323399573677E-16,60.));
#15005=CARTESIAN_POINT('',(5.,-6.12323399573677E-16,60.));
#15006=CARTESIAN_POINT('Origin',(0.,0.,60.));
#15007=CARTESIAN_POINT('Origin',(0.,0.,80.));
#15008=CARTESIAN_POINT('',(3.,-3.67394039744206E-16,60.));
#15009=CARTESIAN_POINT('Origin',(0.,0.,60.));
#15010=CARTESIAN_POINT('',(3.,-3.67394039744206E-16,80.));
#15011=CARTESIAN_POINT('Origin',(0.,0.,60.));
#15012=CARTESIAN_POINT('Origin',(0.,0.,0.));
#15013=CARTESIAN_POINT('Origin',(3.,0.,80.));
#15014=CARTESIAN_POINT('Origin',(-3.,0.,80.));
#15015=CARTESIAN_POINT('',(0.,0.,0.));
#15016=CARTESIAN_POINT('Origin',(0.,0.,12.));
#15017=CARTESIAN_POINT('',(2.,-2.44929359829471E-16,-12.));
#15018=CARTESIAN_POINT('Origin',(0.,0.,-12.));
#15019=CARTESIAN_POINT('',(2.,-2.44929359829471E-16,12.));
#15020=CARTESIAN_POINT('',(2.,-2.44929359829471E-16,12.));
#15021=CARTESIAN_POINT('Origin',(0.,0.,12.));
#15022=CARTESIAN_POINT('Origin',(0.,0.,12.));
#15023=CARTESIAN_POINT('Origin',(0.,0.,-12.));
#15024=CARTESIAN_POINT('',(0.,0.,0.));
#15025=CARTESIAN_POINT('Origin',(32.,3.,115.8875));
#15026=CARTESIAN_POINT('',(32.,3.,121.3875));
#15027=CARTESIAN_POINT('Origin',(32.,3.,115.8875));
#15028=CARTESIAN_POINT('',(32.,0.,121.3875));
#15029=CARTESIAN_POINT('',(32.,3.,121.3875));
#15030=CARTESIAN_POINT('Origin',(32.,0.,115.8875));
#15031=CARTESIAN_POINT('Origin',(-32.,3.,115.8875));
#15032=CARTESIAN_POINT('',(-32.,3.,121.3875));
#15033=CARTESIAN_POINT('Origin',(-32.,3.,115.8875));
#15034=CARTESIAN_POINT('',(-32.,0.,121.3875));
#15035=CARTESIAN_POINT('',(-32.,3.,121.3875));
#15036=CARTESIAN_POINT('Origin',(-32.,0.,115.8875));
#15037=CARTESIAN_POINT('Origin',(-32.,7.,115.8875));
#15038=CARTESIAN_POINT('',(-32.,6.,119.1875));
#15039=CARTESIAN_POINT('Origin',(-32.,6.,115.8875));
#15040=CARTESIAN_POINT('',(-32.,3.,119.1875));
#15041=CARTESIAN_POINT('',(-32.,7.,119.1875));
#15042=CARTESIAN_POINT('Origin',(-32.,3.,115.8875));
#15043=CARTESIAN_POINT('Origin',(32.,7.,115.8875));
#15044=CARTESIAN_POINT('',(32.,6.,119.1875));
#15045=CARTESIAN_POINT('Origin',(32.,6.,115.8875));
#15046=CARTESIAN_POINT('',(32.,3.,119.1875));
#15047=CARTESIAN_POINT('',(32.,7.,119.1875));
#15048=CARTESIAN_POINT('Origin',(32.,3.,115.8875));
#15049=CARTESIAN_POINT('Origin',(50.8,6.,98.425));
#15050=CARTESIAN_POINT('',(50.8,0.,133.35));
#15051=CARTESIAN_POINT('',(50.8,0.,98.425));
#15052=CARTESIAN_POINT('',(50.8,0.,98.425));
#15053=CARTESIAN_POINT('',(50.8,6.,98.425));
#15054=CARTESIAN_POINT('',(50.8,6.,98.425));
#15055=CARTESIAN_POINT('',(50.8,6.,133.35));
#15056=CARTESIAN_POINT('',(50.8,6.,98.425));
#15057=CARTESIAN_POINT('',(50.8,6.,133.35));
#15058=CARTESIAN_POINT('Origin',(-50.8,6.,98.425));
#15059=CARTESIAN_POINT('',(-50.8,0.,98.425));
#15060=CARTESIAN_POINT('',(-50.8,0.,98.425));
#15061=CARTESIAN_POINT('',(-50.8,6.,98.425));
#15062=CARTESIAN_POINT('',(-50.8,6.,98.425));
#15063=CARTESIAN_POINT('',(-50.8,6.,98.425));
#15064=CARTESIAN_POINT('Origin',(-50.8,6.,98.425));
#15065=CARTESIAN_POINT('',(-50.8,0.,133.35));
#15066=CARTESIAN_POINT('',(-50.8,0.,98.425));
#15067=CARTESIAN_POINT('',(-50.8,6.,133.35));
#15068=CARTESIAN_POINT('',(-50.8,6.,133.35));
#15069=CARTESIAN_POINT('',(-50.8,6.,98.425));
#15070=CARTESIAN_POINT('Origin',(-50.8,6.,133.35));
#15071=CARTESIAN_POINT('',(-50.8,0.,133.35));
#15072=CARTESIAN_POINT('',(-50.8,6.,133.35));
#15073=CARTESIAN_POINT('Origin',(0.,6.,0.));
#15074=CARTESIAN_POINT('Origin',(0.,0.,0.));
#15075=CARTESIAN_POINT('Origin',(-32.,3.,115.8875));
#15076=CARTESIAN_POINT('Origin',(32.,3.,115.8875));
#15077=CARTESIAN_POINT('',(0.,0.,0.));
#15078=CARTESIAN_POINT('Origin',(28.,3.,4.));
#15079=CARTESIAN_POINT('',(31.3,3.,4.));
#15080=CARTESIAN_POINT('Origin',(28.,3.,4.));
#15081=CARTESIAN_POINT('',(31.3,3.,0.));
#15082=CARTESIAN_POINT('',(31.3,3.,4.));
#15083=CARTESIAN_POINT('Origin',(28.,3.,0.));
#15084=CARTESIAN_POINT('Origin',(-28.,3.,4.));
#15085=CARTESIAN_POINT('',(-24.7,3.,4.));
#15086=CARTESIAN_POINT('Origin',(-28.,3.,4.));
#15087=CARTESIAN_POINT('',(-24.7,3.,0.));
#15088=CARTESIAN_POINT('',(-24.7,3.,4.));
#15089=CARTESIAN_POINT('Origin',(-28.,3.,0.));
#15090=CARTESIAN_POINT('Origin',(0.,0.,4.));
#15091=CARTESIAN_POINT('',(6.2,-7.59281015471359E-16,4.));
#15092=CARTESIAN_POINT('Origin',(0.,0.,4.));
#15093=CARTESIAN_POINT('',(6.2,-7.59281015471359E-16,5.55111512312578E-16));
#15094=CARTESIAN_POINT('',(6.2,-7.59281015471359E-16,4.));
#15095=CARTESIAN_POINT('Origin',(0.,0.,0.));
#15096=CARTESIAN_POINT('Origin',(0.,0.,4.));
#15097=CARTESIAN_POINT('',(-38.,7.,4.));
#15098=CARTESIAN_POINT('',(-38.,-3.,4.));
#15099=CARTESIAN_POINT('',(-38.,7.,4.));
#15100=CARTESIAN_POINT('',(-31.,-10.,4.));
#15101=CARTESIAN_POINT('',(-38.,-3.,4.));
#15102=CARTESIAN_POINT('',(31.,-10.,4.));
#15103=CARTESIAN_POINT('',(-31.,-10.,4.));
#15104=CARTESIAN_POINT('',(38.,-3.,4.));
#15105=CARTESIAN_POINT('',(31.,-10.,4.));
#15106=CARTESIAN_POINT('',(38.,7.,4.));
#15107=CARTESIAN_POINT('',(38.,-3.,4.));
#15108=CARTESIAN_POINT('',(31.,14.,4.));
#15109=CARTESIAN_POINT('',(38.,7.,4.));
#15110=CARTESIAN_POINT('',(-31.,14.,4.));
#15111=CARTESIAN_POINT('',(31.,14.,4.));
#15112=CARTESIAN_POINT('',(-31.,14.,4.));
#15113=CARTESIAN_POINT('Origin',(0.,0.,0.));
#15114=CARTESIAN_POINT('',(-38.,7.,0.));
#15115=CARTESIAN_POINT('',(-38.,-3.,0.));
#15116=CARTESIAN_POINT('',(-38.,7.,0.));
#15117=CARTESIAN_POINT('',(-31.,14.,0.));
#15118=CARTESIAN_POINT('',(-31.,14.,0.));
#15119=CARTESIAN_POINT('',(31.,14.,0.));
#15120=CARTESIAN_POINT('',(31.,14.,0.));
#15121=CARTESIAN_POINT('',(38.,7.,0.));
#15122=CARTESIAN_POINT('',(38.,7.,0.));
#15123=CARTESIAN_POINT('',(38.,-3.,0.));
#15124=CARTESIAN_POINT('',(38.,-3.,0.));
#15125=CARTESIAN_POINT('',(31.,-10.,0.));
#15126=CARTESIAN_POINT('',(31.,-10.,0.));
#15127=CARTESIAN_POINT('',(-31.,-10.,0.));
#15128=CARTESIAN_POINT('',(-31.,-10.,0.));
#15129=CARTESIAN_POINT('',(-38.,-3.,0.));
#15130=CARTESIAN_POINT('Origin',(-38.,7.,4.));
#15131=CARTESIAN_POINT('',(-38.,-3.,4.));
#15132=CARTESIAN_POINT('',(-38.,7.,4.));
#15133=CARTESIAN_POINT('Origin',(-38.,-3.,4.));
#15134=CARTESIAN_POINT('',(-31.,-10.,4.));
#15135=CARTESIAN_POINT('Origin',(-31.,-10.,4.));
#15136=CARTESIAN_POINT('',(31.,-10.,4.));
#15137=CARTESIAN_POINT('Origin',(31.,-10.,4.));
#15138=CARTESIAN_POINT('',(38.,-3.,4.));
#15139=CARTESIAN_POINT('Origin',(38.,-3.,4.));
#15140=CARTESIAN_POINT('',(38.,7.,4.));
#15141=CARTESIAN_POINT('Origin',(38.,7.,4.));
#15142=CARTESIAN_POINT('',(31.,14.,4.));
#15143=CARTESIAN_POINT('Origin',(31.,14.,4.));
#15144=CARTESIAN_POINT('',(-31.,14.,4.));
#15145=CARTESIAN_POINT('Origin',(-31.,14.,4.));
#15146=CARTESIAN_POINT('',(0.,0.,0.));
#15147=CARTESIAN_POINT('Origin',(0.,0.,22.));
#15148=CARTESIAN_POINT('',(6.2,-7.59281015471359E-16,22.));
#15149=CARTESIAN_POINT('Origin',(0.,0.,22.));
#15150=CARTESIAN_POINT('',(6.2,-7.59281015471359E-16,0.));
#15151=CARTESIAN_POINT('',(6.2,-7.59281015471359E-16,22.));
#15152=CARTESIAN_POINT('Origin',(0.,0.,0.));
#15153=CARTESIAN_POINT('Origin',(0.,0.,22.));
#15154=CARTESIAN_POINT('',(14.,-1.71450551880629E-15,0.));
#15155=CARTESIAN_POINT('Origin',(0.,0.,0.));
#15156=CARTESIAN_POINT('',(14.,-1.71450551880629E-15,1.));
#15157=CARTESIAN_POINT('',(14.,-1.71450551880629E-15,22.));
#15158=CARTESIAN_POINT('',(13.9994857048393,-0.12,1.));
#15159=CARTESIAN_POINT('Origin',(0.,0.,1.));
#15160=CARTESIAN_POINT('',(13.9994857048393,-0.12,7.));
#15161=CARTESIAN_POINT('',(13.9994857048393,-0.12,22.));
#15162=CARTESIAN_POINT('',(14.,-1.71450551880629E-15,7.));
#15163=CARTESIAN_POINT('Origin',(0.,0.,7.));
#15164=CARTESIAN_POINT('',(14.,-1.71450551880629E-15,22.));
#15165=CARTESIAN_POINT('',(14.,-1.71450551880629E-15,22.));
#15166=CARTESIAN_POINT('Origin',(0.,0.,22.));
#15167=CARTESIAN_POINT('',(13.9994857048393,0.12,7.));
#15168=CARTESIAN_POINT('Origin',(0.,0.,7.));
#15169=CARTESIAN_POINT('',(13.9994857048393,0.12,1.));
#15170=CARTESIAN_POINT('',(13.9994857048393,0.12,22.));
#15171=CARTESIAN_POINT('Origin',(0.,0.,1.));
#15172=CARTESIAN_POINT('',(-13.9994857048393,0.120000000000002,7.));
#15173=CARTESIAN_POINT('',(-13.9994857048393,-0.119999999999998,7.));
#15174=CARTESIAN_POINT('Origin',(0.,0.,7.));
#15175=CARTESIAN_POINT('',(-13.9994857048393,-0.119999999999998,1.));
#15176=CARTESIAN_POINT('',(-13.9994857048393,-0.119999999999998,22.));
#15177=CARTESIAN_POINT('',(-13.9994857048393,0.120000000000002,1.));
#15178=CARTESIAN_POINT('Origin',(0.,0.,1.));
#15179=CARTESIAN_POINT('',(-13.9994857048393,0.120000000000002,22.));
#15180=CARTESIAN_POINT('',(9.81427846127362,-9.98398408875839,7.));
#15181=CARTESIAN_POINT('',(9.81427846127362,-9.98398408875839,1.));
#15182=CARTESIAN_POINT('',(9.81427846127362,-9.98398408875839,22.));
#15183=CARTESIAN_POINT('',(9.98398408875839,-9.81427846127362,7.));
#15184=CARTESIAN_POINT('Origin',(0.,0.,7.));
#15185=CARTESIAN_POINT('',(9.98398408875839,-9.81427846127362,1.));
#15186=CARTESIAN_POINT('',(9.98398408875839,-9.81427846127362,22.));
#15187=CARTESIAN_POINT('Origin',(0.,0.,1.));
#15188=CARTESIAN_POINT('',(-0.120000000000003,-13.9994857048393,7.));
#15189=CARTESIAN_POINT('',(-0.120000000000003,-13.9994857048393,1.));
#15190=CARTESIAN_POINT('',(-0.120000000000003,-13.9994857048393,22.));
#15191=CARTESIAN_POINT('',(0.119999999999997,-13.9994857048393,7.));
#15192=CARTESIAN_POINT('Origin',(0.,0.,7.));
#15193=CARTESIAN_POINT('',(0.119999999999997,-13.9994857048393,1.));
#15194=CARTESIAN_POINT('',(0.119999999999997,-13.9994857048393,22.));
#15195=CARTESIAN_POINT('Origin',(0.,0.,1.));
#15196=CARTESIAN_POINT('',(-9.98398408875839,-9.81427846127362,7.));
#15197=CARTESIAN_POINT('',(-9.98398408875839,-9.81427846127362,1.));
#15198=CARTESIAN_POINT('',(-9.98398408875839,-9.81427846127362,22.));
#15199=CARTESIAN_POINT('',(-9.81427846127362,-9.98398408875839,7.));
#15200=CARTESIAN_POINT('Origin',(0.,0.,7.));
#15201=CARTESIAN_POINT('',(-9.81427846127362,-9.98398408875839,1.));
#15202=CARTESIAN_POINT('',(-9.81427846127362,-9.98398408875839,22.));
#15203=CARTESIAN_POINT('Origin',(0.,0.,1.));
#15204=CARTESIAN_POINT('',(13.8083566691933,-2.30852465794632,4.));
#15205=CARTESIAN_POINT('',(13.8083566691933,-2.30852465794632,1.));
#15206=CARTESIAN_POINT('',(13.8083566691933,-2.30852465794632,22.));
#15207=CARTESIAN_POINT('',(13.8459009408029,-2.07147945620348,4.));
#15208=CARTESIAN_POINT('Origin',(0.,0.,4.));
#15209=CARTESIAN_POINT('',(13.8459009408029,-2.07147945620348,1.));
#15210=CARTESIAN_POINT('',(13.8459009408029,-2.07147945620348,22.));
#15211=CARTESIAN_POINT('Origin',(0.,0.,1.));
#15212=CARTESIAN_POINT('',(13.2772200650433,-4.44020577725991,4.));
#15213=CARTESIAN_POINT('',(13.2772200650433,-4.44020577725991,1.));
#15214=CARTESIAN_POINT('',(13.2772200650433,-4.44020577725991,22.));
#15215=CARTESIAN_POINT('',(13.3513841436933,-4.21195221334907,4.));
#15216=CARTESIAN_POINT('Origin',(0.,0.,4.));
#15217=CARTESIAN_POINT('',(13.3513841436933,-4.21195221334907,1.));
#15218=CARTESIAN_POINT('',(13.3513841436933,-4.21195221334907,22.));
#15219=CARTESIAN_POINT('Origin',(0.,0.,1.));
#15220=CARTESIAN_POINT('',(12.4191542383249,-6.46255429413924,4.));
#15221=CARTESIAN_POINT('',(12.4191542383249,-6.46255429413924,1.));
#15222=CARTESIAN_POINT('',(12.4191542383249,-6.46255429413924,22.));
#15223=CARTESIAN_POINT('',(12.5281119582624,-6.24871272833404,4.));
#15224=CARTESIAN_POINT('Origin',(0.,0.,4.));
#15225=CARTESIAN_POINT('',(12.5281119582624,-6.24871272833404,1.));
#15226=CARTESIAN_POINT('',(12.5281119582624,-6.24871272833404,22.));
#15227=CARTESIAN_POINT('Origin',(0.,0.,1.));
#15228=CARTESIAN_POINT('',(11.255287617449,-8.32577327630884,4.));
#15229=CARTESIAN_POINT('',(11.255287617449,-8.32577327630884,1.));
#15230=CARTESIAN_POINT('',(11.255287617449,-8.32577327630884,22.));
#15231=CARTESIAN_POINT('',(11.3963560779992,-8.13160919765885,4.));
#15232=CARTESIAN_POINT('Origin',(0.,0.,4.));
#15233=CARTESIAN_POINT('',(11.3963560779992,-8.13160919765885,1.));
#15234=CARTESIAN_POINT('',(11.3963560779992,-8.13160919765885,22.));
#15235=CARTESIAN_POINT('Origin',(0.,0.,1.));
#15236=CARTESIAN_POINT('',(8.13160919765884,-11.3963560779992,4.));
#15237=CARTESIAN_POINT('',(8.13160919765884,-11.3963560779992,1.));
#15238=CARTESIAN_POINT('',(8.13160919765884,-11.3963560779992,22.));
#15239=CARTESIAN_POINT('',(8.32577327630883,-11.255287617449,4.));
#15240=CARTESIAN_POINT('Origin',(0.,0.,4.));
#15241=CARTESIAN_POINT('',(8.32577327630883,-11.255287617449,1.));
#15242=CARTESIAN_POINT('',(8.32577327630883,-11.255287617449,22.));
#15243=CARTESIAN_POINT('Origin',(0.,0.,1.));
#15244=CARTESIAN_POINT('',(6.24871272833403,-12.5281119582624,4.));
#15245=CARTESIAN_POINT('',(6.24871272833403,-12.5281119582624,1.));
#15246=CARTESIAN_POINT('',(6.24871272833403,-12.5281119582624,22.));
#15247=CARTESIAN_POINT('',(6.46255429413924,-12.4191542383249,4.));
#15248=CARTESIAN_POINT('Origin',(0.,0.,4.));
#15249=CARTESIAN_POINT('',(6.46255429413924,-12.4191542383249,1.));
#15250=CARTESIAN_POINT('',(6.46255429413924,-12.4191542383249,22.));
#15251=CARTESIAN_POINT('Origin',(0.,0.,1.));
#15252=CARTESIAN_POINT('',(4.21195221334906,-13.3513841436933,4.));
#15253=CARTESIAN_POINT('',(4.21195221334906,-13.3513841436933,1.));
#15254=CARTESIAN_POINT('',(4.21195221334906,-13.3513841436933,22.));
#15255=CARTESIAN_POINT('',(4.4402057772599,-13.2772200650433,4.));
#15256=CARTESIAN_POINT('Origin',(0.,0.,4.));
#15257=CARTESIAN_POINT('',(4.4402057772599,-13.2772200650433,1.));
#15258=CARTESIAN_POINT('',(4.4402057772599,-13.2772200650433,22.));
#15259=CARTESIAN_POINT('Origin',(0.,0.,1.));
#15260=CARTESIAN_POINT('',(2.07147945620348,-13.8459009408029,4.));
#15261=CARTESIAN_POINT('',(2.07147945620348,-13.8459009408029,1.));
#15262=CARTESIAN_POINT('',(2.07147945620348,-13.8459009408029,22.));
#15263=CARTESIAN_POINT('',(2.30852465794631,-13.8083566691933,4.));
#15264=CARTESIAN_POINT('Origin',(0.,0.,4.));
#15265=CARTESIAN_POINT('',(2.30852465794631,-13.8083566691933,1.));
#15266=CARTESIAN_POINT('',(2.30852465794631,-13.8083566691933,22.));
#15267=CARTESIAN_POINT('Origin',(0.,0.,1.));
#15268=CARTESIAN_POINT('',(-2.30852465794632,-13.8083566691933,4.));
#15269=CARTESIAN_POINT('',(-2.30852465794632,-13.8083566691933,1.));
#15270=CARTESIAN_POINT('',(-2.30852465794631,-13.8083566691933,22.));
#15271=CARTESIAN_POINT('',(-2.07147945620348,-13.8459009408029,4.));
#15272=CARTESIAN_POINT('Origin',(0.,0.,4.));
#15273=CARTESIAN_POINT('',(-2.07147945620348,-13.8459009408029,1.));
#15274=CARTESIAN_POINT('',(-2.07147945620348,-13.8459009408029,22.));
#15275=CARTESIAN_POINT('Origin',(0.,0.,1.));
#15276=CARTESIAN_POINT('',(-4.44020577725991,-13.2772200650433,4.));
#15277=CARTESIAN_POINT('',(-4.44020577725991,-13.2772200650433,1.));
#15278=CARTESIAN_POINT('',(-4.4402057772599,-13.2772200650433,22.));
#15279=CARTESIAN_POINT('',(-4.21195221334907,-13.3513841436933,4.));
#15280=CARTESIAN_POINT('Origin',(0.,0.,4.));
#15281=CARTESIAN_POINT('',(-4.21195221334907,-13.3513841436933,1.));
#15282=CARTESIAN_POINT('',(-4.21195221334907,-13.3513841436933,22.));
#15283=CARTESIAN_POINT('Origin',(0.,0.,1.));
#15284=CARTESIAN_POINT('',(-6.46255429413924,-12.4191542383249,4.));
#15285=CARTESIAN_POINT('',(-6.46255429413924,-12.4191542383249,1.));
#15286=CARTESIAN_POINT('',(-6.46255429413924,-12.4191542383249,22.));
#15287=CARTESIAN_POINT('',(-6.24871272833404,-12.5281119582624,4.));
#15288=CARTESIAN_POINT('Origin',(0.,0.,4.));
#15289=CARTESIAN_POINT('',(-6.24871272833404,-12.5281119582624,1.));
#15290=CARTESIAN_POINT('',(-6.24871272833404,-12.5281119582624,22.));
#15291=CARTESIAN_POINT('Origin',(0.,0.,1.));
#15292=CARTESIAN_POINT('',(-8.32577327630884,-11.255287617449,4.));
#15293=CARTESIAN_POINT('',(-8.32577327630884,-11.255287617449,1.));
#15294=CARTESIAN_POINT('',(-8.32577327630884,-11.255287617449,22.));
#15295=CARTESIAN_POINT('',(-8.13160919765885,-11.3963560779992,4.));
#15296=CARTESIAN_POINT('Origin',(0.,0.,4.));
#15297=CARTESIAN_POINT('',(-8.13160919765885,-11.3963560779992,1.));
#15298=CARTESIAN_POINT('',(-8.13160919765885,-11.3963560779992,22.));
#15299=CARTESIAN_POINT('Origin',(0.,0.,1.));
#15300=CARTESIAN_POINT('',(-11.3963560779992,-8.13160919765885,4.));
#15301=CARTESIAN_POINT('',(-11.3963560779992,-8.13160919765885,1.));
#15302=CARTESIAN_POINT('',(-11.3963560779992,-8.13160919765885,22.));
#15303=CARTESIAN_POINT('',(-11.255287617449,-8.32577327630884,4.));
#15304=CARTESIAN_POINT('Origin',(0.,0.,4.));
#15305=CARTESIAN_POINT('',(-11.255287617449,-8.32577327630884,1.));
#15306=CARTESIAN_POINT('',(-11.255287617449,-8.32577327630884,22.));
#15307=CARTESIAN_POINT('Origin',(0.,0.,1.));
#15308=CARTESIAN_POINT('',(-12.5281119582624,-6.24871272833403,4.));
#15309=CARTESIAN_POINT('',(-12.5281119582624,-6.24871272833403,1.));
#15310=CARTESIAN_POINT('',(-12.5281119582624,-6.24871272833403,22.));
#15311=CARTESIAN_POINT('',(-12.4191542383249,-6.46255429413924,4.));
#15312=CARTESIAN_POINT('Origin',(0.,0.,4.));
#15313=CARTESIAN_POINT('',(-12.4191542383249,-6.46255429413924,1.));
#15314=CARTESIAN_POINT('',(-12.4191542383249,-6.46255429413924,22.));
#15315=CARTESIAN_POINT('Origin',(0.,0.,1.));
#15316=CARTESIAN_POINT('',(-13.3513841436933,-4.21195221334906,4.));
#15317=CARTESIAN_POINT('',(-13.3513841436933,-4.21195221334906,1.));
#15318=CARTESIAN_POINT('',(-13.3513841436933,-4.21195221334906,22.));
#15319=CARTESIAN_POINT('',(-13.2772200650433,-4.44020577725989,4.));
#15320=CARTESIAN_POINT('Origin',(0.,0.,4.));
#15321=CARTESIAN_POINT('',(-13.2772200650433,-4.44020577725989,1.));
#15322=CARTESIAN_POINT('',(-13.2772200650433,-4.44020577725989,22.));
#15323=CARTESIAN_POINT('Origin',(0.,0.,1.));
#15324=CARTESIAN_POINT('',(-13.8459009408029,-2.07147945620348,4.));
#15325=CARTESIAN_POINT('',(-13.8459009408029,-2.07147945620348,1.));
#15326=CARTESIAN_POINT('',(-13.8459009408029,-2.07147945620348,22.));
#15327=CARTESIAN_POINT('',(-13.8083566691933,-2.30852465794631,4.));
#15328=CARTESIAN_POINT('Origin',(0.,0.,4.));
#15329=CARTESIAN_POINT('',(-13.8083566691933,-2.30852465794631,1.));
#15330=CARTESIAN_POINT('',(-13.8083566691933,-2.30852465794631,22.));
#15331=CARTESIAN_POINT('Origin',(0.,0.,1.));
#15332=CARTESIAN_POINT('',(-9.81427846127362,9.98398408875839,7.));
#15333=CARTESIAN_POINT('',(-9.81427846127362,9.98398408875839,1.));
#15334=CARTESIAN_POINT('',(-9.81427846127362,9.98398408875839,22.));
#15335=CARTESIAN_POINT('',(-9.98398408875839,9.81427846127362,7.));
#15336=CARTESIAN_POINT('Origin',(0.,0.,7.));
#15337=CARTESIAN_POINT('',(-9.98398408875839,9.81427846127362,1.));
#15338=CARTESIAN_POINT('',(-9.98398408875839,9.81427846127362,22.));
#15339=CARTESIAN_POINT('Origin',(0.,0.,1.));
#15340=CARTESIAN_POINT('',(0.120000000000001,13.9994857048393,7.));
#15341=CARTESIAN_POINT('',(0.120000000000001,13.9994857048393,1.));
#15342=CARTESIAN_POINT('',(0.120000000000001,13.9994857048393,22.));
#15343=CARTESIAN_POINT('',(-0.119999999999999,13.9994857048393,7.));
#15344=CARTESIAN_POINT('Origin',(0.,0.,7.));
#15345=CARTESIAN_POINT('',(-0.119999999999999,13.9994857048393,1.));
#15346=CARTESIAN_POINT('',(-0.119999999999999,13.9994857048393,22.));
#15347=CARTESIAN_POINT('Origin',(0.,0.,1.));
#15348=CARTESIAN_POINT('',(9.98398408875839,9.81427846127362,7.));
#15349=CARTESIAN_POINT('',(9.98398408875839,9.81427846127362,1.));
#15350=CARTESIAN_POINT('',(9.98398408875839,9.81427846127362,22.));
#15351=CARTESIAN_POINT('',(9.81427846127362,9.98398408875839,7.));
#15352=CARTESIAN_POINT('Origin',(0.,0.,7.));
#15353=CARTESIAN_POINT('',(9.81427846127362,9.98398408875839,1.));
#15354=CARTESIAN_POINT('',(9.81427846127362,9.98398408875839,22.));
#15355=CARTESIAN_POINT('Origin',(0.,0.,1.));
#15356=CARTESIAN_POINT('',(13.8459009408029,2.07147945620348,4.));
#15357=CARTESIAN_POINT('',(13.8459009408029,2.07147945620348,1.));
#15358=CARTESIAN_POINT('',(13.8459009408029,2.07147945620348,22.));
#15359=CARTESIAN_POINT('',(13.8083566691933,2.30852465794631,4.));
#15360=CARTESIAN_POINT('Origin',(0.,0.,4.));
#15361=CARTESIAN_POINT('',(13.8083566691933,2.30852465794631,1.));
#15362=CARTESIAN_POINT('',(13.8083566691933,2.30852465794631,22.));
#15363=CARTESIAN_POINT('Origin',(0.,0.,1.));
#15364=CARTESIAN_POINT('',(-13.8083566691933,2.30852465794631,4.));
#15365=CARTESIAN_POINT('',(-13.8083566691933,2.30852465794631,1.));
#15366=CARTESIAN_POINT('',(-13.8083566691933,2.30852465794631,22.));
#15367=CARTESIAN_POINT('',(-13.8459009408029,2.07147945620348,4.));
#15368=CARTESIAN_POINT('Origin',(0.,0.,4.));
#15369=CARTESIAN_POINT('',(-13.8459009408029,2.07147945620348,1.));
#15370=CARTESIAN_POINT('',(-13.8459009408029,2.07147945620348,22.));
#15371=CARTESIAN_POINT('Origin',(0.,0.,1.));
#15372=CARTESIAN_POINT('',(-13.2772200650433,4.4402057772599,4.));
#15373=CARTESIAN_POINT('',(-13.2772200650433,4.4402057772599,1.));
#15374=CARTESIAN_POINT('',(-13.2772200650433,4.4402057772599,22.));
#15375=CARTESIAN_POINT('',(-13.3513841436933,4.21195221334907,4.));
#15376=CARTESIAN_POINT('Origin',(0.,0.,4.));
#15377=CARTESIAN_POINT('',(-13.3513841436933,4.21195221334907,1.));
#15378=CARTESIAN_POINT('',(-13.3513841436933,4.21195221334907,22.));
#15379=CARTESIAN_POINT('Origin',(0.,0.,1.));
#15380=CARTESIAN_POINT('',(-12.4191542383249,6.46255429413924,4.));
#15381=CARTESIAN_POINT('',(-12.4191542383249,6.46255429413924,1.));
#15382=CARTESIAN_POINT('',(-12.4191542383249,6.46255429413924,22.));
#15383=CARTESIAN_POINT('',(-12.5281119582624,6.24871272833403,4.));
#15384=CARTESIAN_POINT('Origin',(0.,0.,4.));
#15385=CARTESIAN_POINT('',(-12.5281119582624,6.24871272833403,1.));
#15386=CARTESIAN_POINT('',(-12.5281119582624,6.24871272833403,22.));
#15387=CARTESIAN_POINT('Origin',(0.,0.,1.));
#15388=CARTESIAN_POINT('',(-11.255287617449,8.32577327630884,4.));
#15389=CARTESIAN_POINT('',(-11.255287617449,8.32577327630884,1.));
#15390=CARTESIAN_POINT('',(-11.255287617449,8.32577327630884,22.));
#15391=CARTESIAN_POINT('',(-11.3963560779992,8.13160919765885,4.));
#15392=CARTESIAN_POINT('Origin',(0.,0.,4.));
#15393=CARTESIAN_POINT('',(-11.3963560779992,8.13160919765885,1.));
#15394=CARTESIAN_POINT('',(-11.3963560779992,8.13160919765885,22.));
#15395=CARTESIAN_POINT('Origin',(0.,0.,1.));
#15396=CARTESIAN_POINT('',(-8.13160919765885,11.3963560779992,4.));
#15397=CARTESIAN_POINT('',(-8.13160919765885,11.3963560779992,1.));
#15398=CARTESIAN_POINT('',(-8.13160919765885,11.3963560779992,22.));
#15399=CARTESIAN_POINT('',(-8.32577327630884,11.255287617449,4.));
#15400=CARTESIAN_POINT('Origin',(0.,0.,4.));
#15401=CARTESIAN_POINT('',(-8.32577327630884,11.255287617449,1.));
#15402=CARTESIAN_POINT('',(-8.32577327630884,11.255287617449,22.));
#15403=CARTESIAN_POINT('Origin',(0.,0.,1.));
#15404=CARTESIAN_POINT('',(-6.24871272833403,12.5281119582624,4.));
#15405=CARTESIAN_POINT('',(-6.24871272833403,12.5281119582624,1.));
#15406=CARTESIAN_POINT('',(-6.24871272833403,12.5281119582624,22.));
#15407=CARTESIAN_POINT('',(-6.46255429413924,12.4191542383249,4.));
#15408=CARTESIAN_POINT('Origin',(0.,0.,4.));
#15409=CARTESIAN_POINT('',(-6.46255429413924,12.4191542383249,1.));
#15410=CARTESIAN_POINT('',(-6.46255429413924,12.4191542383249,22.));
#15411=CARTESIAN_POINT('Origin',(0.,0.,1.));
#15412=CARTESIAN_POINT('',(-4.21195221334906,13.3513841436933,4.));
#15413=CARTESIAN_POINT('',(-4.21195221334906,13.3513841436933,1.));
#15414=CARTESIAN_POINT('',(-4.21195221334906,13.3513841436933,22.));
#15415=CARTESIAN_POINT('',(-4.4402057772599,13.2772200650433,4.));
#15416=CARTESIAN_POINT('Origin',(0.,0.,4.));
#15417=CARTESIAN_POINT('',(-4.4402057772599,13.2772200650433,1.));
#15418=CARTESIAN_POINT('',(-4.4402057772599,13.2772200650433,22.));
#15419=CARTESIAN_POINT('Origin',(0.,0.,1.));
#15420=CARTESIAN_POINT('',(-2.07147945620348,13.8459009408029,4.));
#15421=CARTESIAN_POINT('',(-2.07147945620348,13.8459009408029,1.));
#15422=CARTESIAN_POINT('',(-2.07147945620348,13.8459009408029,22.));
#15423=CARTESIAN_POINT('',(-2.30852465794631,13.8083566691933,4.));
#15424=CARTESIAN_POINT('Origin',(0.,0.,4.));
#15425=CARTESIAN_POINT('',(-2.30852465794631,13.8083566691933,1.));
#15426=CARTESIAN_POINT('',(-2.30852465794631,13.8083566691933,22.));
#15427=CARTESIAN_POINT('Origin',(0.,0.,1.));
#15428=CARTESIAN_POINT('',(2.30852465794631,13.8083566691933,4.));
#15429=CARTESIAN_POINT('',(2.30852465794631,13.8083566691933,1.));
#15430=CARTESIAN_POINT('',(2.30852465794631,13.8083566691933,22.));
#15431=CARTESIAN_POINT('',(2.07147945620348,13.8459009408029,4.));
#15432=CARTESIAN_POINT('Origin',(0.,0.,4.));
#15433=CARTESIAN_POINT('',(2.07147945620348,13.8459009408029,1.));
#15434=CARTESIAN_POINT('',(2.07147945620348,13.8459009408029,22.));
#15435=CARTESIAN_POINT('Origin',(0.,0.,1.));
#15436=CARTESIAN_POINT('',(4.4402057772599,13.2772200650433,4.));
#15437=CARTESIAN_POINT('',(4.4402057772599,13.2772200650433,1.));
#15438=CARTESIAN_POINT('',(4.4402057772599,13.2772200650433,22.));
#15439=CARTESIAN_POINT('',(4.21195221334907,13.3513841436933,4.));
#15440=CARTESIAN_POINT('Origin',(0.,0.,4.));
#15441=CARTESIAN_POINT('',(4.21195221334907,13.3513841436933,1.));
#15442=CARTESIAN_POINT('',(4.21195221334907,13.3513841436933,22.));
#15443=CARTESIAN_POINT('Origin',(0.,0.,1.));
#15444=CARTESIAN_POINT('',(6.46255429413924,12.4191542383249,4.));
#15445=CARTESIAN_POINT('',(6.46255429413924,12.4191542383249,1.));
#15446=CARTESIAN_POINT('',(6.46255429413924,12.4191542383249,22.));
#15447=CARTESIAN_POINT('',(6.24871272833403,12.5281119582624,4.));
#15448=CARTESIAN_POINT('Origin',(0.,0.,4.));
#15449=CARTESIAN_POINT('',(6.24871272833403,12.5281119582624,1.));
#15450=CARTESIAN_POINT('',(6.24871272833403,12.5281119582624,22.));
#15451=CARTESIAN_POINT('Origin',(0.,0.,1.));
#15452=CARTESIAN_POINT('',(8.32577327630884,11.255287617449,4.));
#15453=CARTESIAN_POINT('',(8.32577327630884,11.255287617449,1.));
#15454=CARTESIAN_POINT('',(8.32577327630884,11.255287617449,22.));
#15455=CARTESIAN_POINT('',(8.13160919765885,11.3963560779992,4.));
#15456=CARTESIAN_POINT('Origin',(0.,0.,4.));
#15457=CARTESIAN_POINT('',(8.13160919765885,11.3963560779992,1.));
#15458=CARTESIAN_POINT('',(8.13160919765885,11.3963560779992,22.));
#15459=CARTESIAN_POINT('Origin',(0.,0.,1.));
#15460=CARTESIAN_POINT('',(11.3963560779992,8.13160919765885,4.));
#15461=CARTESIAN_POINT('',(11.3963560779992,8.13160919765885,1.));
#15462=CARTESIAN_POINT('',(11.3963560779992,8.13160919765885,22.));
#15463=CARTESIAN_POINT('',(11.255287617449,8.32577327630884,4.));
#15464=CARTESIAN_POINT('Origin',(0.,0.,4.));
#15465=CARTESIAN_POINT('',(11.255287617449,8.32577327630884,1.));
#15466=CARTESIAN_POINT('',(11.255287617449,8.32577327630884,22.));
#15467=CARTESIAN_POINT('Origin',(0.,0.,1.));
#15468=CARTESIAN_POINT('',(12.5281119582624,6.24871272833403,4.));
#15469=CARTESIAN_POINT('',(12.5281119582624,6.24871272833403,1.));
#15470=CARTESIAN_POINT('',(12.5281119582624,6.24871272833403,22.));
#15471=CARTESIAN_POINT('',(12.4191542383249,6.46255429413924,4.));
#15472=CARTESIAN_POINT('Origin',(0.,0.,4.));
#15473=CARTESIAN_POINT('',(12.4191542383249,6.46255429413924,1.));
#15474=CARTESIAN_POINT('',(12.4191542383249,6.46255429413924,22.));
#15475=CARTESIAN_POINT('Origin',(0.,0.,1.));
#15476=CARTESIAN_POINT('',(13.3513841436933,4.21195221334907,4.));
#15477=CARTESIAN_POINT('',(13.3513841436933,4.21195221334907,1.));
#15478=CARTESIAN_POINT('',(13.3513841436933,4.21195221334907,22.));
#15479=CARTESIAN_POINT('',(13.2772200650433,4.4402057772599,4.));
#15480=CARTESIAN_POINT('Origin',(0.,0.,4.));
#15481=CARTESIAN_POINT('',(13.2772200650433,4.4402057772599,1.));
#15482=CARTESIAN_POINT('',(13.2772200650433,4.4402057772599,22.));
#15483=CARTESIAN_POINT('Origin',(0.,0.,1.));
#15484=CARTESIAN_POINT('Origin',(0.,0.,22.));
#15485=CARTESIAN_POINT('Origin',(0.,0.,0.));
#15486=CARTESIAN_POINT('Origin',(9.461088732276,-9.63079435976078,7.));
#15487=CARTESIAN_POINT('',(9.461088732276,-9.63079435976078,1.));
#15488=CARTESIAN_POINT('',(9.461088732276,-9.63079435976078,1.));
#15489=CARTESIAN_POINT('',(9.461088732276,-9.63079435976078,7.));
#15490=CARTESIAN_POINT('',(9.461088732276,-9.63079435976078,7.));
#15491=CARTESIAN_POINT('',(9.461088732276,-9.63079435976078,7.));
#15492=CARTESIAN_POINT('Origin',(10.2671904628287,-10.0974848353439,7.));
#15493=CARTESIAN_POINT('',(9.63079435976077,-9.46108873227601,7.));
#15494=CARTESIAN_POINT('',(10.2671904628287,-10.0974848353439,7.));
#15495=CARTESIAN_POINT('',(9.63079435976077,-9.46108873227601,1.));
#15496=CARTESIAN_POINT('',(9.63079435976077,-9.46108873227601,7.));
#15497=CARTESIAN_POINT('',(10.2671904628287,-10.0974848353439,1.));
#15498=CARTESIAN_POINT('Origin',(0.,0.,7.));
#15499=CARTESIAN_POINT('',(9.63079435976077,-9.46108873227601,7.));
#15500=CARTESIAN_POINT('Origin',(0.,0.,1.));
#15501=CARTESIAN_POINT('',(9.63079435976077,-9.46108873227601,1.));
#15502=CARTESIAN_POINT('Origin',(9.63079435976077,-9.46108873227601,7.));
#15503=CARTESIAN_POINT('Origin',(-0.120000000000002,-13.5,7.));
#15504=CARTESIAN_POINT('',(-0.120000000000002,-13.5,1.));
#15505=CARTESIAN_POINT('',(-0.120000000000002,-13.5,1.));
#15506=CARTESIAN_POINT('',(-0.120000000000002,-13.5,7.));
#15507=CARTESIAN_POINT('',(-0.120000000000002,-13.5,7.));
#15508=CARTESIAN_POINT('',(-0.120000000000002,-13.5,7.));
#15509=CARTESIAN_POINT('Origin',(0.119999999999997,-14.4,7.));
#15510=CARTESIAN_POINT('',(0.119999999999998,-13.5,7.));
#15511=CARTESIAN_POINT('',(0.119999999999997,-14.4,7.));
#15512=CARTESIAN_POINT('',(0.119999999999998,-13.5,1.));
#15513=CARTESIAN_POINT('',(0.119999999999998,-13.5,7.));
#15514=CARTESIAN_POINT('',(0.119999999999997,-14.4,1.));
#15515=CARTESIAN_POINT('Origin',(0.,0.,7.));
#15516=CARTESIAN_POINT('',(0.119999999999998,-13.5,7.));
#15517=CARTESIAN_POINT('Origin',(0.,0.,1.));
#15518=CARTESIAN_POINT('',(0.119999999999998,-13.5,1.));
#15519=CARTESIAN_POINT('Origin',(0.119999999999998,-13.5,7.));
#15520=CARTESIAN_POINT('Origin',(-9.63079435976078,-9.46108873227601,7.));
#15521=CARTESIAN_POINT('',(-9.63079435976078,-9.46108873227601,1.));
#15522=CARTESIAN_POINT('',(-9.63079435976078,-9.46108873227601,1.));
#15523=CARTESIAN_POINT('',(-9.63079435976078,-9.46108873227601,7.));
#15524=CARTESIAN_POINT('',(-9.63079435976078,-9.46108873227601,7.));
#15525=CARTESIAN_POINT('',(-9.63079435976078,-9.46108873227601,7.));
#15526=CARTESIAN_POINT('Origin',(-10.0974848353439,-10.2671904628287,7.));
#15527=CARTESIAN_POINT('',(-9.46108873227601,-9.63079435976078,7.));
#15528=CARTESIAN_POINT('',(-10.0974848353439,-10.2671904628287,7.));
#15529=CARTESIAN_POINT('',(-9.46108873227601,-9.63079435976078,1.));
#15530=CARTESIAN_POINT('',(-9.46108873227601,-9.63079435976078,7.));
#15531=CARTESIAN_POINT('',(-10.0974848353439,-10.2671904628287,1.));
#15532=CARTESIAN_POINT('Origin',(0.,0.,7.));
#15533=CARTESIAN_POINT('',(-9.46108873227601,-9.63079435976078,7.));
#15534=CARTESIAN_POINT('Origin',(0.,0.,1.));
#15535=CARTESIAN_POINT('',(-9.46108873227601,-9.63079435976078,1.));
#15536=CARTESIAN_POINT('Origin',(-9.46108873227601,-9.63079435976078,7.));
#15537=CARTESIAN_POINT('Origin',(-13.5,0.120000000000002,7.));
#15538=CARTESIAN_POINT('',(-13.5,0.120000000000002,1.));
#15539=CARTESIAN_POINT('',(-13.5,0.120000000000002,1.));
#15540=CARTESIAN_POINT('',(-13.5,0.120000000000002,7.));
#15541=CARTESIAN_POINT('',(-13.5,0.120000000000002,7.));
#15542=CARTESIAN_POINT('',(-13.5,0.120000000000002,7.));
#15543=CARTESIAN_POINT('Origin',(-14.4,-0.119999999999998,7.));
#15544=CARTESIAN_POINT('',(-13.5,-0.119999999999998,7.));
#15545=CARTESIAN_POINT('',(-14.4,-0.119999999999998,7.));
#15546=CARTESIAN_POINT('',(-13.5,-0.119999999999998,1.));
#15547=CARTESIAN_POINT('',(-13.5,-0.119999999999998,7.));
#15548=CARTESIAN_POINT('',(-14.4,-0.119999999999998,1.));
#15549=CARTESIAN_POINT('Origin',(0.,0.,7.));
#15550=CARTESIAN_POINT('',(-13.5,-0.119999999999998,7.));
#15551=CARTESIAN_POINT('Origin',(0.,0.,1.));
#15552=CARTESIAN_POINT('',(-13.5,-0.119999999999998,1.));
#15553=CARTESIAN_POINT('Origin',(-13.5,-0.119999999999998,7.));
#15554=CARTESIAN_POINT('Origin',(-9.46108873227601,9.63079435976078,7.));
#15555=CARTESIAN_POINT('',(-9.46108873227601,9.63079435976078,1.));
#15556=CARTESIAN_POINT('',(-9.46108873227601,9.63079435976078,1.));
#15557=CARTESIAN_POINT('',(-9.46108873227601,9.63079435976078,7.));
#15558=CARTESIAN_POINT('',(-9.46108873227601,9.63079435976078,7.));
#15559=CARTESIAN_POINT('',(-9.46108873227601,9.63079435976078,7.));
#15560=CARTESIAN_POINT('Origin',(-10.2671904628287,10.0974848353439,7.));
#15561=CARTESIAN_POINT('',(-9.63079435976078,9.46108873227601,7.));
#15562=CARTESIAN_POINT('',(-10.2671904628287,10.0974848353439,7.));
#15563=CARTESIAN_POINT('',(-9.63079435976078,9.46108873227601,1.));
#15564=CARTESIAN_POINT('',(-9.63079435976078,9.46108873227601,7.));
#15565=CARTESIAN_POINT('',(-10.2671904628287,10.0974848353439,1.));
#15566=CARTESIAN_POINT('Origin',(0.,0.,7.));
#15567=CARTESIAN_POINT('',(-9.63079435976078,9.46108873227601,7.));
#15568=CARTESIAN_POINT('Origin',(0.,0.,1.));
#15569=CARTESIAN_POINT('',(-9.63079435976078,9.46108873227601,1.));
#15570=CARTESIAN_POINT('Origin',(-9.63079435976078,9.46108873227601,7.));
#15571=CARTESIAN_POINT('Origin',(0.120000000000001,13.5,7.));
#15572=CARTESIAN_POINT('',(0.120000000000001,13.5,1.));
#15573=CARTESIAN_POINT('',(0.120000000000001,13.5,1.));
#15574=CARTESIAN_POINT('',(0.120000000000001,13.5,7.));
#15575=CARTESIAN_POINT('',(0.120000000000001,13.5,7.));
#15576=CARTESIAN_POINT('',(0.120000000000001,13.5,7.));
#15577=CARTESIAN_POINT('Origin',(-0.119999999999999,14.4,7.));
#15578=CARTESIAN_POINT('',(-0.119999999999999,13.5,7.));
#15579=CARTESIAN_POINT('',(-0.119999999999999,14.4,7.));
#15580=CARTESIAN_POINT('',(-0.119999999999999,13.5,1.));
#15581=CARTESIAN_POINT('',(-0.119999999999999,13.5,7.));
#15582=CARTESIAN_POINT('',(-0.119999999999999,14.4,1.));
#15583=CARTESIAN_POINT('Origin',(0.,0.,7.));
#15584=CARTESIAN_POINT('',(-0.119999999999999,13.5,7.));
#15585=CARTESIAN_POINT('Origin',(0.,0.,1.));
#15586=CARTESIAN_POINT('',(-0.119999999999999,13.5,1.));
#15587=CARTESIAN_POINT('Origin',(-0.119999999999999,13.5,7.));
#15588=CARTESIAN_POINT('Origin',(9.63079435976078,9.46108873227601,7.));
#15589=CARTESIAN_POINT('',(9.63079435976078,9.46108873227601,1.));
#15590=CARTESIAN_POINT('',(9.63079435976078,9.46108873227601,1.));
#15591=CARTESIAN_POINT('',(9.63079435976078,9.46108873227601,7.));
#15592=CARTESIAN_POINT('',(9.63079435976078,9.46108873227601,7.));
#15593=CARTESIAN_POINT('',(9.63079435976078,9.46108873227601,7.));
#15594=CARTESIAN_POINT('Origin',(10.0974848353439,10.2671904628287,7.));
#15595=CARTESIAN_POINT('',(9.46108873227601,9.63079435976078,7.));
#15596=CARTESIAN_POINT('',(10.0974848353439,10.2671904628287,7.));
#15597=CARTESIAN_POINT('',(9.46108873227601,9.63079435976078,1.));
#15598=CARTESIAN_POINT('',(9.46108873227601,9.63079435976078,7.));
#15599=CARTESIAN_POINT('',(10.0974848353439,10.2671904628287,1.));
#15600=CARTESIAN_POINT('Origin',(0.,0.,7.));
#15601=CARTESIAN_POINT('',(9.46108873227601,9.63079435976078,7.));
#15602=CARTESIAN_POINT('Origin',(0.,0.,1.));
#15603=CARTESIAN_POINT('',(9.46108873227601,9.63079435976078,1.));
#15604=CARTESIAN_POINT('Origin',(9.46108873227601,9.63079435976078,7.));
#15605=CARTESIAN_POINT('Origin',(13.5,-0.12,7.));
#15606=CARTESIAN_POINT('',(13.5,-0.12,1.));
#15607=CARTESIAN_POINT('',(13.5,-0.12,1.));
#15608=CARTESIAN_POINT('',(13.5,-0.12,7.));
#15609=CARTESIAN_POINT('',(13.5,-0.12,7.));
#15610=CARTESIAN_POINT('',(13.5,-0.12,7.));
#15611=CARTESIAN_POINT('Origin',(14.4,0.12,7.));
#15612=CARTESIAN_POINT('',(13.5,0.12,7.));
#15613=CARTESIAN_POINT('',(14.4,0.12,7.));
#15614=CARTESIAN_POINT('',(13.5,0.12,1.));
#15615=CARTESIAN_POINT('',(13.5,0.12,7.));
#15616=CARTESIAN_POINT('',(14.4,0.12,1.));
#15617=CARTESIAN_POINT('Origin',(0.,0.,7.));
#15618=CARTESIAN_POINT('',(13.5,0.12,7.));
#15619=CARTESIAN_POINT('Origin',(0.,0.,1.));
#15620=CARTESIAN_POINT('',(13.5,0.12,1.));
#15621=CARTESIAN_POINT('Origin',(13.5,0.12,7.));
#15622=CARTESIAN_POINT('Origin',(13.3525647338392,1.9933426771717,4.));
#15623=CARTESIAN_POINT('',(13.3525647338392,1.9933426771717,1.));
#15624=CARTESIAN_POINT('',(13.3525647338392,1.9933426771717,1.));
#15625=CARTESIAN_POINT('',(13.3525647338392,1.9933426771717,4.));
#15626=CARTESIAN_POINT('',(13.3525647338392,1.9933426771717,4.));
#15627=CARTESIAN_POINT('',(13.3525647338392,1.9933426771717,4.));
#15628=CARTESIAN_POINT('Origin',(14.2039399687652,2.37117889745074,4.));
#15629=CARTESIAN_POINT('',(13.3150204622295,2.23038787891453,4.));
#15630=CARTESIAN_POINT('',(14.2039399687652,2.37117889745074,4.));
#15631=CARTESIAN_POINT('',(13.3150204622295,2.23038787891453,1.));
#15632=CARTESIAN_POINT('',(13.3150204622295,2.23038787891453,4.));
#15633=CARTESIAN_POINT('',(14.2039399687652,2.37117889745074,1.));
#15634=CARTESIAN_POINT('Origin',(0.,0.,4.));
#15635=CARTESIAN_POINT('',(13.3150204622295,2.23038787891453,4.));
#15636=CARTESIAN_POINT('Origin',(0.,0.,1.));
#15637=CARTESIAN_POINT('',(13.3150204622295,2.23038787891453,1.));
#15638=CARTESIAN_POINT('Origin',(13.3150204622295,2.23038787891453,4.));
#15639=CARTESIAN_POINT('Origin',(13.3150204622295,-2.23038787891454,4.));
#15640=CARTESIAN_POINT('',(13.3150204622295,-2.23038787891454,1.));
#15641=CARTESIAN_POINT('',(13.3150204622295,-2.23038787891454,1.));
#15642=CARTESIAN_POINT('',(13.3150204622295,-2.23038787891454,4.));
#15643=CARTESIAN_POINT('',(13.3150204622295,-2.23038787891454,4.));
#15644=CARTESIAN_POINT('',(13.3150204622295,-2.23038787891454,4.));
#15645=CARTESIAN_POINT('Origin',(14.2414842403748,-2.13413369570791,4.));
#15646=CARTESIAN_POINT('',(13.3525647338392,-1.9933426771717,4.));
#15647=CARTESIAN_POINT('',(14.2414842403748,-2.13413369570791,4.));
#15648=CARTESIAN_POINT('',(13.3525647338392,-1.9933426771717,1.));
#15649=CARTESIAN_POINT('',(13.3525647338392,-1.9933426771717,4.));
#15650=CARTESIAN_POINT('',(14.2414842403748,-2.13413369570791,1.));
#15651=CARTESIAN_POINT('Origin',(0.,0.,4.));
#15652=CARTESIAN_POINT('',(13.3525647338392,-1.9933426771717,4.));
#15653=CARTESIAN_POINT('Origin',(0.,0.,1.));
#15654=CARTESIAN_POINT('',(13.3525647338392,-1.9933426771717,1.));
#15655=CARTESIAN_POINT('Origin',(13.3525647338392,-1.9933426771717,4.));
#15656=CARTESIAN_POINT('Origin',(12.8021809306596,-4.28585620601721,4.));
#15657=CARTESIAN_POINT('',(12.8021809306596,-4.28585620601721,1.));
#15658=CARTESIAN_POINT('',(12.8021809306596,-4.28585620601721,1.));
#15659=CARTESIAN_POINT('',(12.8021809306596,-4.28585620601721,4.));
#15660=CARTESIAN_POINT('',(12.8021809306596,-4.28585620601721,4.));
#15661=CARTESIAN_POINT('',(12.8021809306596,-4.28585620601721,4.));
#15662=CARTESIAN_POINT('Origin',(13.7322958739752,-4.33571793704383,4.));
#15663=CARTESIAN_POINT('',(12.8763450093096,-4.05760264210638,4.));
#15664=CARTESIAN_POINT('',(13.7322958739752,-4.33571793704383,4.));
#15665=CARTESIAN_POINT('',(12.8763450093096,-4.05760264210638,1.));
#15666=CARTESIAN_POINT('',(12.8763450093096,-4.05760264210638,4.));
#15667=CARTESIAN_POINT('',(13.7322958739752,-4.33571793704383,1.));
#15668=CARTESIAN_POINT('Origin',(0.,0.,4.));
#15669=CARTESIAN_POINT('',(12.8763450093096,-4.05760264210638,4.));
#15670=CARTESIAN_POINT('Origin',(0.,0.,1.));
#15671=CARTESIAN_POINT('',(12.8763450093096,-4.05760264210638,1.));
#15672=CARTESIAN_POINT('Origin',(12.8763450093096,-4.05760264210638,4.));
#15673=CARTESIAN_POINT('Origin',(11.9741092165742,-6.23579252938649,4.));
#15674=CARTESIAN_POINT('',(11.9741092165742,-6.23579252938649,1.));
#15675=CARTESIAN_POINT('',(11.9741092165742,-6.23579252938649,1.));
#15676=CARTESIAN_POINT('',(11.9741092165742,-6.23579252938649,4.));
#15677=CARTESIAN_POINT('',(11.9741092165742,-6.23579252938649,4.));
#15678=CARTESIAN_POINT('',(11.9741092165742,-6.23579252938649,4.));
#15679=CARTESIAN_POINT('Origin',(12.8849728082812,-6.43054241334687,4.));
#15680=CARTESIAN_POINT('',(12.0830669365117,-6.02195096358128,4.));
#15681=CARTESIAN_POINT('',(12.8849728082812,-6.43054241334687,4.));
#15682=CARTESIAN_POINT('',(12.0830669365117,-6.02195096358128,1.));
#15683=CARTESIAN_POINT('',(12.0830669365117,-6.02195096358128,4.));
#15684=CARTESIAN_POINT('',(12.8849728082812,-6.43054241334687,1.));
#15685=CARTESIAN_POINT('Origin',(0.,0.,4.));
#15686=CARTESIAN_POINT('',(12.0830669365117,-6.02195096358128,4.));
#15687=CARTESIAN_POINT('Origin',(0.,0.,1.));
#15688=CARTESIAN_POINT('',(12.0830669365117,-6.02195096358128,1.));
#15689=CARTESIAN_POINT('Origin',(12.0830669365117,-6.02195096358128,4.));
#15690=CARTESIAN_POINT('Origin',(10.8511951937867,-8.03218294527338,4.));
#15691=CARTESIAN_POINT('',(10.8511951937867,-8.03218294527338,1.));
#15692=CARTESIAN_POINT('',(10.8511951937867,-8.03218294527338,1.));
#15693=CARTESIAN_POINT('',(10.8511951937867,-8.03218294527338,4.));
#15694=CARTESIAN_POINT('',(10.8511951937867,-8.03218294527338,4.));
#15695=CARTESIAN_POINT('',(10.8511951937867,-8.03218294527338,4.));
#15696=CARTESIAN_POINT('Origin',(11.7203789492743,-8.36702559368663,4.));
#15697=CARTESIAN_POINT('',(10.9922636543369,-7.8380188666234,4.));
#15698=CARTESIAN_POINT('',(11.7203789492743,-8.36702559368663,4.));
#15699=CARTESIAN_POINT('',(10.9922636543369,-7.8380188666234,1.));
#15700=CARTESIAN_POINT('',(10.9922636543369,-7.8380188666234,4.));
#15701=CARTESIAN_POINT('',(11.7203789492743,-8.36702559368663,1.));
#15702=CARTESIAN_POINT('Origin',(0.,0.,4.));
#15703=CARTESIAN_POINT('',(10.9922636543369,-7.8380188666234,4.));
#15704=CARTESIAN_POINT('Origin',(0.,0.,1.));
#15705=CARTESIAN_POINT('',(10.9922636543369,-7.8380188666234,1.));
#15706=CARTESIAN_POINT('Origin',(10.9922636543369,-7.8380188666234,4.));
#15707=CARTESIAN_POINT('Origin',(7.83801886662339,-10.9922636543369,4.));
#15708=CARTESIAN_POINT('',(7.83801886662339,-10.9922636543369,1.));
#15709=CARTESIAN_POINT('',(7.83801886662339,-10.9922636543369,1.));
#15710=CARTESIAN_POINT('',(7.83801886662339,-10.9922636543369,4.));
#15711=CARTESIAN_POINT('',(7.83801886662339,-10.9922636543369,4.));
#15712=CARTESIAN_POINT('',(7.83801886662339,-10.9922636543369,4.));
#15713=CARTESIAN_POINT('Origin',(8.5611896723366,-11.5793104887241,4.));
#15714=CARTESIAN_POINT('',(8.03218294527338,-10.8511951937867,4.));
#15715=CARTESIAN_POINT('',(8.5611896723366,-11.5793104887241,4.));
#15716=CARTESIAN_POINT('',(8.03218294527338,-10.8511951937867,1.));
#15717=CARTESIAN_POINT('',(8.03218294527338,-10.8511951937867,4.));
#15718=CARTESIAN_POINT('',(8.5611896723366,-11.5793104887241,1.));
#15719=CARTESIAN_POINT('Origin',(0.,0.,4.));
#15720=CARTESIAN_POINT('',(8.03218294527338,-10.8511951937867,4.));
#15721=CARTESIAN_POINT('Origin',(0.,0.,1.));
#15722=CARTESIAN_POINT('',(8.03218294527338,-10.8511951937867,1.));
#15723=CARTESIAN_POINT('Origin',(8.03218294527338,-10.8511951937867,4.));
#15724=CARTESIAN_POINT('Origin',(6.02195096358128,-12.0830669365117,4.));
#15725=CARTESIAN_POINT('',(6.02195096358128,-12.0830669365117,1.));
#15726=CARTESIAN_POINT('',(6.02195096358128,-12.0830669365117,1.));
#15727=CARTESIAN_POINT('',(6.02195096358128,-12.0830669365117,4.));
#15728=CARTESIAN_POINT('',(6.02195096358128,-12.0830669365117,4.));
#15729=CARTESIAN_POINT('',(6.02195096358128,-12.0830669365117,4.));
#15730=CARTESIAN_POINT('Origin',(6.64438397915208,-12.7760150883438,4.));
#15731=CARTESIAN_POINT('',(6.23579252938648,-11.9741092165742,4.));
#15732=CARTESIAN_POINT('',(6.64438397915208,-12.7760150883438,4.));
#15733=CARTESIAN_POINT('',(6.23579252938648,-11.9741092165742,1.));
#15734=CARTESIAN_POINT('',(6.23579252938648,-11.9741092165742,4.));
#15735=CARTESIAN_POINT('',(6.64438397915208,-12.7760150883438,1.));
#15736=CARTESIAN_POINT('Origin',(0.,0.,4.));
#15737=CARTESIAN_POINT('',(6.23579252938648,-11.9741092165742,4.));
#15738=CARTESIAN_POINT('Origin',(0.,0.,1.));
#15739=CARTESIAN_POINT('',(6.23579252938648,-11.9741092165742,1.));
#15740=CARTESIAN_POINT('Origin',(6.23579252938648,-11.9741092165742,4.));
#15741=CARTESIAN_POINT('Origin',(4.05760264210637,-12.8763450093096,4.));
#15742=CARTESIAN_POINT('',(4.05760264210637,-12.8763450093096,1.));
#15743=CARTESIAN_POINT('',(4.05760264210637,-12.8763450093096,1.));
#15744=CARTESIAN_POINT('',(4.05760264210637,-12.8763450093096,4.));
#15745=CARTESIAN_POINT('',(4.05760264210637,-12.8763450093096,4.));
#15746=CARTESIAN_POINT('',(4.05760264210637,-12.8763450093096,4.));
#15747=CARTESIAN_POINT('Origin',(4.56397150095466,-13.6581317953252,4.));
#15748=CARTESIAN_POINT('',(4.28585620601721,-12.8021809306596,4.));
#15749=CARTESIAN_POINT('',(4.56397150095466,-13.6581317953252,4.));
#15750=CARTESIAN_POINT('',(4.28585620601721,-12.8021809306596,1.));
#15751=CARTESIAN_POINT('',(4.28585620601721,-12.8021809306596,4.));
#15752=CARTESIAN_POINT('',(4.56397150095466,-13.6581317953252,1.));
#15753=CARTESIAN_POINT('Origin',(0.,0.,4.));
#15754=CARTESIAN_POINT('',(4.28585620601721,-12.8021809306596,4.));
#15755=CARTESIAN_POINT('Origin',(0.,0.,1.));
#15756=CARTESIAN_POINT('',(4.28585620601721,-12.8021809306596,1.));
#15757=CARTESIAN_POINT('Origin',(4.28585620601721,-12.8021809306596,4.));
#15758=CARTESIAN_POINT('Origin',(1.9933426771717,-13.3525647338392,4.));
#15759=CARTESIAN_POINT('',(1.9933426771717,-13.3525647338392,1.));
#15760=CARTESIAN_POINT('',(1.9933426771717,-13.3525647338392,1.));
#15761=CARTESIAN_POINT('',(1.9933426771717,-13.3525647338392,4.));
#15762=CARTESIAN_POINT('',(1.9933426771717,-13.3525647338392,4.));
#15763=CARTESIAN_POINT('',(1.9933426771717,-13.3525647338392,4.));
#15764=CARTESIAN_POINT('Origin',(2.37117889745074,-14.2039399687652,4.));
#15765=CARTESIAN_POINT('',(2.23038787891453,-13.3150204622295,4.));
#15766=CARTESIAN_POINT('',(2.37117889745074,-14.2039399687652,4.));
#15767=CARTESIAN_POINT('',(2.23038787891453,-13.3150204622295,1.));
#15768=CARTESIAN_POINT('',(2.23038787891453,-13.3150204622295,4.));
#15769=CARTESIAN_POINT('',(2.37117889745074,-14.2039399687652,1.));
#15770=CARTESIAN_POINT('Origin',(0.,0.,4.));
#15771=CARTESIAN_POINT('',(2.23038787891453,-13.3150204622295,4.));
#15772=CARTESIAN_POINT('Origin',(0.,0.,1.));
#15773=CARTESIAN_POINT('',(2.23038787891453,-13.3150204622295,1.));
#15774=CARTESIAN_POINT('Origin',(2.23038787891453,-13.3150204622295,4.));
#15775=CARTESIAN_POINT('Origin',(-2.23038787891454,-13.3150204622295,4.));
#15776=CARTESIAN_POINT('',(-2.23038787891454,-13.3150204622295,1.));
#15777=CARTESIAN_POINT('',(-2.23038787891454,-13.3150204622295,1.));
#15778=CARTESIAN_POINT('',(-2.23038787891454,-13.3150204622295,4.));
#15779=CARTESIAN_POINT('',(-2.23038787891454,-13.3150204622295,4.));
#15780=CARTESIAN_POINT('',(-2.23038787891454,-13.3150204622295,4.));
#15781=CARTESIAN_POINT('Origin',(-2.13413369570791,-14.2414842403748,4.));
#15782=CARTESIAN_POINT('',(-1.9933426771717,-13.3525647338392,4.));
#15783=CARTESIAN_POINT('',(-2.13413369570791,-14.2414842403748,4.));
#15784=CARTESIAN_POINT('',(-1.9933426771717,-13.3525647338392,1.));
#15785=CARTESIAN_POINT('',(-1.9933426771717,-13.3525647338392,4.));
#15786=CARTESIAN_POINT('',(-2.13413369570791,-14.2414842403748,1.));
#15787=CARTESIAN_POINT('Origin',(0.,0.,4.));
#15788=CARTESIAN_POINT('',(-1.9933426771717,-13.3525647338392,4.));
#15789=CARTESIAN_POINT('Origin',(0.,0.,1.));
#15790=CARTESIAN_POINT('',(-1.9933426771717,-13.3525647338392,1.));
#15791=CARTESIAN_POINT('Origin',(-1.9933426771717,-13.3525647338392,4.));
#15792=CARTESIAN_POINT('Origin',(-4.28585620601721,-12.8021809306596,4.));
#15793=CARTESIAN_POINT('',(-4.28585620601721,-12.8021809306596,1.));
#15794=CARTESIAN_POINT('',(-4.28585620601721,-12.8021809306596,1.));
#15795=CARTESIAN_POINT('',(-4.28585620601721,-12.8021809306596,4.));
#15796=CARTESIAN_POINT('',(-4.28585620601721,-12.8021809306596,4.));
#15797=CARTESIAN_POINT('',(-4.28585620601721,-12.8021809306596,4.));
#15798=CARTESIAN_POINT('Origin',(-4.33571793704383,-13.7322958739752,4.));
#15799=CARTESIAN_POINT('',(-4.05760264210637,-12.8763450093096,4.));
#15800=CARTESIAN_POINT('',(-4.33571793704383,-13.7322958739752,4.));
#15801=CARTESIAN_POINT('',(-4.05760264210637,-12.8763450093096,1.));
#15802=CARTESIAN_POINT('',(-4.05760264210637,-12.8763450093096,4.));
#15803=CARTESIAN_POINT('',(-4.33571793704383,-13.7322958739752,1.));
#15804=CARTESIAN_POINT('Origin',(0.,0.,4.));
#15805=CARTESIAN_POINT('',(-4.05760264210637,-12.8763450093096,4.));
#15806=CARTESIAN_POINT('Origin',(0.,0.,1.));
#15807=CARTESIAN_POINT('',(-4.05760264210637,-12.8763450093096,1.));
#15808=CARTESIAN_POINT('Origin',(-4.05760264210637,-12.8763450093096,4.));
#15809=CARTESIAN_POINT('Origin',(-6.23579252938649,-11.9741092165742,4.));
#15810=CARTESIAN_POINT('',(-6.23579252938649,-11.9741092165742,1.));
#15811=CARTESIAN_POINT('',(-6.23579252938649,-11.9741092165742,1.));
#15812=CARTESIAN_POINT('',(-6.23579252938649,-11.9741092165742,4.));
#15813=CARTESIAN_POINT('',(-6.23579252938649,-11.9741092165742,4.));
#15814=CARTESIAN_POINT('',(-6.23579252938649,-11.9741092165742,4.));
#15815=CARTESIAN_POINT('Origin',(-6.43054241334687,-12.8849728082812,4.));
#15816=CARTESIAN_POINT('',(-6.02195096358128,-12.0830669365117,4.));
#15817=CARTESIAN_POINT('',(-6.43054241334687,-12.8849728082812,4.));
#15818=CARTESIAN_POINT('',(-6.02195096358128,-12.0830669365117,1.));
#15819=CARTESIAN_POINT('',(-6.02195096358128,-12.0830669365117,4.));
#15820=CARTESIAN_POINT('',(-6.43054241334687,-12.8849728082812,1.));
#15821=CARTESIAN_POINT('Origin',(0.,0.,4.));
#15822=CARTESIAN_POINT('',(-6.02195096358128,-12.0830669365117,4.));
#15823=CARTESIAN_POINT('Origin',(0.,0.,1.));
#15824=CARTESIAN_POINT('',(-6.02195096358128,-12.0830669365117,1.));
#15825=CARTESIAN_POINT('Origin',(-6.02195096358128,-12.0830669365117,4.));
#15826=CARTESIAN_POINT('Origin',(-8.03218294527338,-10.8511951937867,4.));
#15827=CARTESIAN_POINT('',(-8.03218294527338,-10.8511951937867,1.));
#15828=CARTESIAN_POINT('',(-8.03218294527338,-10.8511951937867,1.));
#15829=CARTESIAN_POINT('',(-8.03218294527338,-10.8511951937867,4.));
#15830=CARTESIAN_POINT('',(-8.03218294527338,-10.8511951937867,4.));
#15831=CARTESIAN_POINT('',(-8.03218294527338,-10.8511951937867,4.));
#15832=CARTESIAN_POINT('Origin',(-8.36702559368662,-11.7203789492743,4.));
#15833=CARTESIAN_POINT('',(-7.8380188666234,-10.9922636543369,4.));
#15834=CARTESIAN_POINT('',(-8.36702559368662,-11.7203789492743,4.));
#15835=CARTESIAN_POINT('',(-7.8380188666234,-10.9922636543369,1.));
#15836=CARTESIAN_POINT('',(-7.8380188666234,-10.9922636543369,4.));
#15837=CARTESIAN_POINT('',(-8.36702559368662,-11.7203789492743,1.));
#15838=CARTESIAN_POINT('Origin',(0.,0.,4.));
#15839=CARTESIAN_POINT('',(-7.8380188666234,-10.9922636543369,4.));
#15840=CARTESIAN_POINT('Origin',(0.,0.,1.));
#15841=CARTESIAN_POINT('',(-7.8380188666234,-10.9922636543369,1.));
#15842=CARTESIAN_POINT('Origin',(-7.8380188666234,-10.9922636543369,4.));
#15843=CARTESIAN_POINT('Origin',(-10.9922636543369,-7.83801886662339,4.));
#15844=CARTESIAN_POINT('',(-10.9922636543369,-7.83801886662339,1.));
#15845=CARTESIAN_POINT('',(-10.9922636543369,-7.83801886662339,1.));
#15846=CARTESIAN_POINT('',(-10.9922636543369,-7.83801886662339,4.));
#15847=CARTESIAN_POINT('',(-10.9922636543369,-7.83801886662339,4.));
#15848=CARTESIAN_POINT('',(-10.9922636543369,-7.83801886662339,4.));
#15849=CARTESIAN_POINT('Origin',(-11.5793104887241,-8.5611896723366,4.));
#15850=CARTESIAN_POINT('',(-10.8511951937867,-8.03218294527338,4.));
#15851=CARTESIAN_POINT('',(-11.5793104887241,-8.5611896723366,4.));
#15852=CARTESIAN_POINT('',(-10.8511951937867,-8.03218294527338,1.));
#15853=CARTESIAN_POINT('',(-10.8511951937867,-8.03218294527338,4.));
#15854=CARTESIAN_POINT('',(-11.5793104887241,-8.5611896723366,1.));
#15855=CARTESIAN_POINT('Origin',(0.,0.,4.));
#15856=CARTESIAN_POINT('',(-10.8511951937867,-8.03218294527338,4.));
#15857=CARTESIAN_POINT('Origin',(0.,0.,1.));
#15858=CARTESIAN_POINT('',(-10.8511951937867,-8.03218294527338,1.));
#15859=CARTESIAN_POINT('Origin',(-10.8511951937867,-8.03218294527338,4.));
#15860=CARTESIAN_POINT('Origin',(-12.0830669365117,-6.02195096358128,4.));
#15861=CARTESIAN_POINT('',(-12.0830669365117,-6.02195096358128,1.));
#15862=CARTESIAN_POINT('',(-12.0830669365117,-6.02195096358128,1.));
#15863=CARTESIAN_POINT('',(-12.0830669365117,-6.02195096358128,4.));
#15864=CARTESIAN_POINT('',(-12.0830669365117,-6.02195096358128,4.));
#15865=CARTESIAN_POINT('',(-12.0830669365117,-6.02195096358128,4.));
#15866=CARTESIAN_POINT('Origin',(-12.7760150883438,-6.64438397915208,4.));
#15867=CARTESIAN_POINT('',(-11.9741092165742,-6.23579252938648,4.));
#15868=CARTESIAN_POINT('',(-12.7760150883438,-6.64438397915208,4.));
#15869=CARTESIAN_POINT('',(-11.9741092165742,-6.23579252938648,1.));
#15870=CARTESIAN_POINT('',(-11.9741092165742,-6.23579252938648,4.));
#15871=CARTESIAN_POINT('',(-12.7760150883438,-6.64438397915208,1.));
#15872=CARTESIAN_POINT('Origin',(0.,0.,4.));
#15873=CARTESIAN_POINT('',(-11.9741092165742,-6.23579252938648,4.));
#15874=CARTESIAN_POINT('Origin',(0.,0.,1.));
#15875=CARTESIAN_POINT('',(-11.9741092165742,-6.23579252938648,1.));
#15876=CARTESIAN_POINT('Origin',(-11.9741092165742,-6.23579252938648,4.));
#15877=CARTESIAN_POINT('Origin',(-12.8763450093096,-4.05760264210636,4.));
#15878=CARTESIAN_POINT('',(-12.8763450093096,-4.05760264210636,1.));
#15879=CARTESIAN_POINT('',(-12.8763450093096,-4.05760264210636,1.));
#15880=CARTESIAN_POINT('',(-12.8763450093096,-4.05760264210636,4.));
#15881=CARTESIAN_POINT('',(-12.8763450093096,-4.05760264210636,4.));
#15882=CARTESIAN_POINT('',(-12.8763450093096,-4.05760264210636,4.));
#15883=CARTESIAN_POINT('Origin',(-13.6581317953252,-4.56397150095465,4.));
#15884=CARTESIAN_POINT('',(-12.8021809306596,-4.2858562060172,4.));
#15885=CARTESIAN_POINT('',(-13.6581317953252,-4.56397150095465,4.));
#15886=CARTESIAN_POINT('',(-12.8021809306596,-4.2858562060172,1.));
#15887=CARTESIAN_POINT('',(-12.8021809306596,-4.2858562060172,4.));
#15888=CARTESIAN_POINT('',(-13.6581317953252,-4.56397150095465,1.));
#15889=CARTESIAN_POINT('Origin',(0.,0.,4.));
#15890=CARTESIAN_POINT('',(-12.8021809306596,-4.2858562060172,4.));
#15891=CARTESIAN_POINT('Origin',(0.,0.,1.));
#15892=CARTESIAN_POINT('',(-12.8021809306596,-4.2858562060172,1.));
#15893=CARTESIAN_POINT('Origin',(-12.8021809306596,-4.2858562060172,4.));
#15894=CARTESIAN_POINT('Origin',(-13.3525647338392,-1.9933426771717,4.));
#15895=CARTESIAN_POINT('',(-13.3525647338392,-1.9933426771717,1.));
#15896=CARTESIAN_POINT('',(-13.3525647338392,-1.9933426771717,1.));
#15897=CARTESIAN_POINT('',(-13.3525647338392,-1.9933426771717,4.));
#15898=CARTESIAN_POINT('',(-13.3525647338392,-1.9933426771717,4.));
#15899=CARTESIAN_POINT('',(-13.3525647338392,-1.9933426771717,4.));
#15900=CARTESIAN_POINT('Origin',(-14.2039399687652,-2.37117889745074,4.));
#15901=CARTESIAN_POINT('',(-13.3150204622295,-2.23038787891453,4.));
#15902=CARTESIAN_POINT('',(-14.2039399687652,-2.37117889745074,4.));
#15903=CARTESIAN_POINT('',(-13.3150204622295,-2.23038787891453,1.));
#15904=CARTESIAN_POINT('',(-13.3150204622295,-2.23038787891453,4.));
#15905=CARTESIAN_POINT('',(-14.2039399687652,-2.37117889745074,1.));
#15906=CARTESIAN_POINT('Origin',(0.,0.,4.));
#15907=CARTESIAN_POINT('',(-13.3150204622295,-2.23038787891453,4.));
#15908=CARTESIAN_POINT('Origin',(0.,0.,1.));
#15909=CARTESIAN_POINT('',(-13.3150204622295,-2.23038787891453,1.));
#15910=CARTESIAN_POINT('Origin',(-13.3150204622295,-2.23038787891453,4.));
#15911=CARTESIAN_POINT('Origin',(-13.3150204622295,2.23038787891453,4.));
#15912=CARTESIAN_POINT('',(-13.3150204622295,2.23038787891453,1.));
#15913=CARTESIAN_POINT('',(-13.3150204622295,2.23038787891453,1.));
#15914=CARTESIAN_POINT('',(-13.3150204622295,2.23038787891453,4.));
#15915=CARTESIAN_POINT('',(-13.3150204622295,2.23038787891453,4.));
#15916=CARTESIAN_POINT('',(-13.3150204622295,2.23038787891453,4.));
#15917=CARTESIAN_POINT('Origin',(-14.2414842403748,2.13413369570791,4.));
#15918=CARTESIAN_POINT('',(-13.3525647338392,1.9933426771717,4.));
#15919=CARTESIAN_POINT('',(-14.2414842403748,2.13413369570791,4.));
#15920=CARTESIAN_POINT('',(-13.3525647338392,1.9933426771717,1.));
#15921=CARTESIAN_POINT('',(-13.3525647338392,1.9933426771717,4.));
#15922=CARTESIAN_POINT('',(-14.2414842403748,2.13413369570791,1.));
#15923=CARTESIAN_POINT('Origin',(0.,0.,4.));
#15924=CARTESIAN_POINT('',(-13.3525647338392,1.9933426771717,4.));
#15925=CARTESIAN_POINT('Origin',(0.,0.,1.));
#15926=CARTESIAN_POINT('',(-13.3525647338392,1.9933426771717,1.));
#15927=CARTESIAN_POINT('Origin',(-13.3525647338392,1.9933426771717,4.));
#15928=CARTESIAN_POINT('Origin',(-12.8021809306596,4.28585620601721,4.));
#15929=CARTESIAN_POINT('',(-12.8021809306596,4.28585620601721,1.));
#15930=CARTESIAN_POINT('',(-12.8021809306596,4.28585620601721,1.));
#15931=CARTESIAN_POINT('',(-12.8021809306596,4.28585620601721,4.));
#15932=CARTESIAN_POINT('',(-12.8021809306596,4.28585620601721,4.));
#15933=CARTESIAN_POINT('',(-12.8021809306596,4.28585620601721,4.));
#15934=CARTESIAN_POINT('Origin',(-13.7322958739752,4.33571793704383,4.));
#15935=CARTESIAN_POINT('',(-12.8763450093096,4.05760264210637,4.));
#15936=CARTESIAN_POINT('',(-13.7322958739752,4.33571793704383,4.));
#15937=CARTESIAN_POINT('',(-12.8763450093096,4.05760264210637,1.));
#15938=CARTESIAN_POINT('',(-12.8763450093096,4.05760264210637,4.));
#15939=CARTESIAN_POINT('',(-13.7322958739752,4.33571793704383,1.));
#15940=CARTESIAN_POINT('Origin',(0.,0.,4.));
#15941=CARTESIAN_POINT('',(-12.8763450093096,4.05760264210637,4.));
#15942=CARTESIAN_POINT('Origin',(0.,0.,1.));
#15943=CARTESIAN_POINT('',(-12.8763450093096,4.05760264210637,1.));
#15944=CARTESIAN_POINT('Origin',(-12.8763450093096,4.05760264210637,4.));
#15945=CARTESIAN_POINT('Origin',(-11.9741092165742,6.23579252938649,4.));
#15946=CARTESIAN_POINT('',(-11.9741092165742,6.23579252938649,1.));
#15947=CARTESIAN_POINT('',(-11.9741092165742,6.23579252938649,1.));
#15948=CARTESIAN_POINT('',(-11.9741092165742,6.23579252938649,4.));
#15949=CARTESIAN_POINT('',(-11.9741092165742,6.23579252938649,4.));
#15950=CARTESIAN_POINT('',(-11.9741092165742,6.23579252938649,4.));
#15951=CARTESIAN_POINT('Origin',(-12.8849728082812,6.43054241334687,4.));
#15952=CARTESIAN_POINT('',(-12.0830669365117,6.02195096358128,4.));
#15953=CARTESIAN_POINT('',(-12.8849728082812,6.43054241334687,4.));
#15954=CARTESIAN_POINT('',(-12.0830669365117,6.02195096358128,1.));
#15955=CARTESIAN_POINT('',(-12.0830669365117,6.02195096358128,4.));
#15956=CARTESIAN_POINT('',(-12.8849728082812,6.43054241334687,1.));
#15957=CARTESIAN_POINT('Origin',(0.,0.,4.));
#15958=CARTESIAN_POINT('',(-12.0830669365117,6.02195096358128,4.));
#15959=CARTESIAN_POINT('Origin',(0.,0.,1.));
#15960=CARTESIAN_POINT('',(-12.0830669365117,6.02195096358128,1.));
#15961=CARTESIAN_POINT('Origin',(-12.0830669365117,6.02195096358128,4.));
#15962=CARTESIAN_POINT('Origin',(-10.8511951937867,8.03218294527338,4.));
#15963=CARTESIAN_POINT('',(-10.8511951937867,8.03218294527338,1.));
#15964=CARTESIAN_POINT('',(-10.8511951937867,8.03218294527338,1.));
#15965=CARTESIAN_POINT('',(-10.8511951937867,8.03218294527338,4.));
#15966=CARTESIAN_POINT('',(-10.8511951937867,8.03218294527338,4.));
#15967=CARTESIAN_POINT('',(-10.8511951937867,8.03218294527338,4.));
#15968=CARTESIAN_POINT('Origin',(-11.7203789492743,8.36702559368662,4.));
#15969=CARTESIAN_POINT('',(-10.9922636543369,7.8380188666234,4.));
#15970=CARTESIAN_POINT('',(-11.7203789492743,8.36702559368662,4.));
#15971=CARTESIAN_POINT('',(-10.9922636543369,7.8380188666234,1.));
#15972=CARTESIAN_POINT('',(-10.9922636543369,7.8380188666234,4.));
#15973=CARTESIAN_POINT('',(-11.7203789492743,8.36702559368662,1.));
#15974=CARTESIAN_POINT('Origin',(0.,0.,4.));
#15975=CARTESIAN_POINT('',(-10.9922636543369,7.8380188666234,4.));
#15976=CARTESIAN_POINT('Origin',(0.,0.,1.));
#15977=CARTESIAN_POINT('',(-10.9922636543369,7.8380188666234,1.));
#15978=CARTESIAN_POINT('Origin',(-10.9922636543369,7.8380188666234,4.));
#15979=CARTESIAN_POINT('Origin',(-7.83801886662339,10.9922636543369,4.));
#15980=CARTESIAN_POINT('',(-7.83801886662339,10.9922636543369,1.));
#15981=CARTESIAN_POINT('',(-7.83801886662339,10.9922636543369,1.));
#15982=CARTESIAN_POINT('',(-7.83801886662339,10.9922636543369,4.));
#15983=CARTESIAN_POINT('',(-7.83801886662339,10.9922636543369,4.));
#15984=CARTESIAN_POINT('',(-7.83801886662339,10.9922636543369,4.));
#15985=CARTESIAN_POINT('Origin',(-8.5611896723366,11.5793104887241,4.));
#15986=CARTESIAN_POINT('',(-8.03218294527338,10.8511951937867,4.));
#15987=CARTESIAN_POINT('',(-8.5611896723366,11.5793104887241,4.));
#15988=CARTESIAN_POINT('',(-8.03218294527338,10.8511951937867,1.));
#15989=CARTESIAN_POINT('',(-8.03218294527338,10.8511951937867,4.));
#15990=CARTESIAN_POINT('',(-8.5611896723366,11.5793104887241,1.));
#15991=CARTESIAN_POINT('Origin',(0.,0.,4.));
#15992=CARTESIAN_POINT('',(-8.03218294527338,10.8511951937867,4.));
#15993=CARTESIAN_POINT('Origin',(0.,0.,1.));
#15994=CARTESIAN_POINT('',(-8.03218294527338,10.8511951937867,1.));
#15995=CARTESIAN_POINT('Origin',(-8.03218294527338,10.8511951937867,4.));
#15996=CARTESIAN_POINT('Origin',(-6.02195096358128,12.0830669365117,4.));
#15997=CARTESIAN_POINT('',(-6.02195096358128,12.0830669365117,1.));
#15998=CARTESIAN_POINT('',(-6.02195096358128,12.0830669365117,1.));
#15999=CARTESIAN_POINT('',(-6.02195096358128,12.0830669365117,4.));
#16000=CARTESIAN_POINT('',(-6.02195096358128,12.0830669365117,4.));
#16001=CARTESIAN_POINT('',(-6.02195096358128,12.0830669365117,4.));
#16002=CARTESIAN_POINT('Origin',(-6.64438397915208,12.7760150883438,4.));
#16003=CARTESIAN_POINT('',(-6.23579252938649,11.9741092165742,4.));
#16004=CARTESIAN_POINT('',(-6.64438397915208,12.7760150883438,4.));
#16005=CARTESIAN_POINT('',(-6.23579252938649,11.9741092165742,1.));
#16006=CARTESIAN_POINT('',(-6.23579252938649,11.9741092165742,4.));
#16007=CARTESIAN_POINT('',(-6.64438397915208,12.7760150883438,1.));
#16008=CARTESIAN_POINT('Origin',(0.,0.,4.));
#16009=CARTESIAN_POINT('',(-6.23579252938649,11.9741092165742,4.));
#16010=CARTESIAN_POINT('Origin',(0.,0.,1.));
#16011=CARTESIAN_POINT('',(-6.23579252938649,11.9741092165742,1.));
#16012=CARTESIAN_POINT('Origin',(-6.23579252938649,11.9741092165742,4.));
#16013=CARTESIAN_POINT('Origin',(-4.05760264210637,12.8763450093096,4.));
#16014=CARTESIAN_POINT('',(-4.05760264210637,12.8763450093096,1.));
#16015=CARTESIAN_POINT('',(-4.05760264210637,12.8763450093096,1.));
#16016=CARTESIAN_POINT('',(-4.05760264210637,12.8763450093096,4.));
#16017=CARTESIAN_POINT('',(-4.05760264210637,12.8763450093096,4.));
#16018=CARTESIAN_POINT('',(-4.05760264210637,12.8763450093096,4.));
#16019=CARTESIAN_POINT('Origin',(-4.56397150095466,13.6581317953252,4.));
#16020=CARTESIAN_POINT('',(-4.28585620601721,12.8021809306596,4.));
#16021=CARTESIAN_POINT('',(-4.56397150095466,13.6581317953252,4.));
#16022=CARTESIAN_POINT('',(-4.28585620601721,12.8021809306596,1.));
#16023=CARTESIAN_POINT('',(-4.28585620601721,12.8021809306596,4.));
#16024=CARTESIAN_POINT('',(-4.56397150095466,13.6581317953252,1.));
#16025=CARTESIAN_POINT('Origin',(0.,0.,4.));
#16026=CARTESIAN_POINT('',(-4.28585620601721,12.8021809306596,4.));
#16027=CARTESIAN_POINT('Origin',(0.,0.,1.));
#16028=CARTESIAN_POINT('',(-4.28585620601721,12.8021809306596,1.));
#16029=CARTESIAN_POINT('Origin',(-4.28585620601721,12.8021809306596,4.));
#16030=CARTESIAN_POINT('Origin',(-1.9933426771717,13.3525647338392,4.));
#16031=CARTESIAN_POINT('',(-1.9933426771717,13.3525647338392,1.));
#16032=CARTESIAN_POINT('',(-1.9933426771717,13.3525647338392,1.));
#16033=CARTESIAN_POINT('',(-1.9933426771717,13.3525647338392,4.));
#16034=CARTESIAN_POINT('',(-1.9933426771717,13.3525647338392,4.));
#16035=CARTESIAN_POINT('',(-1.9933426771717,13.3525647338392,4.));
#16036=CARTESIAN_POINT('Origin',(-2.37117889745074,14.2039399687652,4.));
#16037=CARTESIAN_POINT('',(-2.23038787891453,13.3150204622295,4.));
#16038=CARTESIAN_POINT('',(-2.37117889745074,14.2039399687652,4.));
#16039=CARTESIAN_POINT('',(-2.23038787891453,13.3150204622295,1.));
#16040=CARTESIAN_POINT('',(-2.23038787891453,13.3150204622295,4.));
#16041=CARTESIAN_POINT('',(-2.37117889745074,14.2039399687652,1.));
#16042=CARTESIAN_POINT('Origin',(0.,0.,4.));
#16043=CARTESIAN_POINT('',(-2.23038787891453,13.3150204622295,4.));
#16044=CARTESIAN_POINT('Origin',(0.,0.,1.));
#16045=CARTESIAN_POINT('',(-2.23038787891453,13.3150204622295,1.));
#16046=CARTESIAN_POINT('Origin',(-2.23038787891453,13.3150204622295,4.));
#16047=CARTESIAN_POINT('Origin',(2.23038787891453,13.3150204622295,4.));
#16048=CARTESIAN_POINT('',(2.23038787891453,13.3150204622295,1.));
#16049=CARTESIAN_POINT('',(2.23038787891453,13.3150204622295,1.));
#16050=CARTESIAN_POINT('',(2.23038787891453,13.3150204622295,4.));
#16051=CARTESIAN_POINT('',(2.23038787891453,13.3150204622295,4.));
#16052=CARTESIAN_POINT('',(2.23038787891453,13.3150204622295,4.));
#16053=CARTESIAN_POINT('Origin',(2.13413369570791,14.2414842403748,4.));
#16054=CARTESIAN_POINT('',(1.9933426771717,13.3525647338392,4.));
#16055=CARTESIAN_POINT('',(2.13413369570791,14.2414842403748,4.));
#16056=CARTESIAN_POINT('',(1.9933426771717,13.3525647338392,1.));
#16057=CARTESIAN_POINT('',(1.9933426771717,13.3525647338392,4.));
#16058=CARTESIAN_POINT('',(2.13413369570791,14.2414842403748,1.));
#16059=CARTESIAN_POINT('Origin',(0.,0.,4.));
#16060=CARTESIAN_POINT('',(1.9933426771717,13.3525647338392,4.));
#16061=CARTESIAN_POINT('Origin',(0.,0.,1.));
#16062=CARTESIAN_POINT('',(1.9933426771717,13.3525647338392,1.));
#16063=CARTESIAN_POINT('Origin',(1.9933426771717,13.3525647338392,4.));
#16064=CARTESIAN_POINT('Origin',(4.28585620601721,12.8021809306596,4.));
#16065=CARTESIAN_POINT('',(4.28585620601721,12.8021809306596,1.));
#16066=CARTESIAN_POINT('',(4.28585620601721,12.8021809306596,1.));
#16067=CARTESIAN_POINT('',(4.28585620601721,12.8021809306596,4.));
#16068=CARTESIAN_POINT('',(4.28585620601721,12.8021809306596,4.));
#16069=CARTESIAN_POINT('',(4.28585620601721,12.8021809306596,4.));
#16070=CARTESIAN_POINT('Origin',(4.33571793704383,13.7322958739752,4.));
#16071=CARTESIAN_POINT('',(4.05760264210637,12.8763450093096,4.));
#16072=CARTESIAN_POINT('',(4.33571793704383,13.7322958739752,4.));
#16073=CARTESIAN_POINT('',(4.05760264210637,12.8763450093096,1.));
#16074=CARTESIAN_POINT('',(4.05760264210637,12.8763450093096,4.));
#16075=CARTESIAN_POINT('',(4.33571793704383,13.7322958739752,1.));
#16076=CARTESIAN_POINT('Origin',(0.,0.,4.));
#16077=CARTESIAN_POINT('',(4.05760264210637,12.8763450093096,4.));
#16078=CARTESIAN_POINT('Origin',(0.,0.,1.));
#16079=CARTESIAN_POINT('',(4.05760264210637,12.8763450093096,1.));
#16080=CARTESIAN_POINT('Origin',(4.05760264210637,12.8763450093096,4.));
#16081=CARTESIAN_POINT('Origin',(6.23579252938649,11.9741092165742,4.));
#16082=CARTESIAN_POINT('',(6.23579252938649,11.9741092165742,1.));
#16083=CARTESIAN_POINT('',(6.23579252938649,11.9741092165742,1.));
#16084=CARTESIAN_POINT('',(6.23579252938649,11.9741092165742,4.));
#16085=CARTESIAN_POINT('',(6.23579252938649,11.9741092165742,4.));
#16086=CARTESIAN_POINT('',(6.23579252938649,11.9741092165742,4.));
#16087=CARTESIAN_POINT('Origin',(6.43054241334687,12.8849728082812,4.));
#16088=CARTESIAN_POINT('',(6.02195096358128,12.0830669365117,4.));
#16089=CARTESIAN_POINT('',(6.43054241334687,12.8849728082812,4.));
#16090=CARTESIAN_POINT('',(6.02195096358128,12.0830669365117,1.));
#16091=CARTESIAN_POINT('',(6.02195096358128,12.0830669365117,4.));
#16092=CARTESIAN_POINT('',(6.43054241334687,12.8849728082812,1.));
#16093=CARTESIAN_POINT('Origin',(0.,0.,4.));
#16094=CARTESIAN_POINT('',(6.02195096358128,12.0830669365117,4.));
#16095=CARTESIAN_POINT('Origin',(0.,0.,1.));
#16096=CARTESIAN_POINT('',(6.02195096358128,12.0830669365117,1.));
#16097=CARTESIAN_POINT('Origin',(6.02195096358128,12.0830669365117,4.));
#16098=CARTESIAN_POINT('Origin',(8.03218294527338,10.8511951937867,4.));
#16099=CARTESIAN_POINT('',(8.03218294527338,10.8511951937867,1.));
#16100=CARTESIAN_POINT('',(8.03218294527338,10.8511951937867,1.));
#16101=CARTESIAN_POINT('',(8.03218294527338,10.8511951937867,4.));
#16102=CARTESIAN_POINT('',(8.03218294527338,10.8511951937867,4.));
#16103=CARTESIAN_POINT('',(8.03218294527338,10.8511951937867,4.));
#16104=CARTESIAN_POINT('Origin',(8.36702559368662,11.7203789492743,4.));
#16105=CARTESIAN_POINT('',(7.8380188666234,10.9922636543369,4.));
#16106=CARTESIAN_POINT('',(8.36702559368662,11.7203789492743,4.));
#16107=CARTESIAN_POINT('',(7.8380188666234,10.9922636543369,1.));
#16108=CARTESIAN_POINT('',(7.8380188666234,10.9922636543369,4.));
#16109=CARTESIAN_POINT('',(8.36702559368662,11.7203789492743,1.));
#16110=CARTESIAN_POINT('Origin',(0.,0.,4.));
#16111=CARTESIAN_POINT('',(7.8380188666234,10.9922636543369,4.));
#16112=CARTESIAN_POINT('Origin',(0.,0.,1.));
#16113=CARTESIAN_POINT('',(7.8380188666234,10.9922636543369,1.));
#16114=CARTESIAN_POINT('Origin',(7.8380188666234,10.9922636543369,4.));
#16115=CARTESIAN_POINT('Origin',(10.9922636543369,7.8380188666234,4.));
#16116=CARTESIAN_POINT('',(10.9922636543369,7.8380188666234,1.));
#16117=CARTESIAN_POINT('',(10.9922636543369,7.8380188666234,1.));
#16118=CARTESIAN_POINT('',(10.9922636543369,7.8380188666234,4.));
#16119=CARTESIAN_POINT('',(10.9922636543369,7.8380188666234,4.));
#16120=CARTESIAN_POINT('',(10.9922636543369,7.8380188666234,4.));
#16121=CARTESIAN_POINT('Origin',(11.5793104887241,8.56118967233661,4.));
#16122=CARTESIAN_POINT('',(10.8511951937867,8.03218294527338,4.));
#16123=CARTESIAN_POINT('',(11.5793104887241,8.56118967233661,4.));
#16124=CARTESIAN_POINT('',(10.8511951937867,8.03218294527338,1.));
#16125=CARTESIAN_POINT('',(10.8511951937867,8.03218294527338,4.));
#16126=CARTESIAN_POINT('',(11.5793104887241,8.56118967233661,1.));
#16127=CARTESIAN_POINT('Origin',(0.,0.,4.));
#16128=CARTESIAN_POINT('',(10.8511951937867,8.03218294527338,4.));
#16129=CARTESIAN_POINT('Origin',(0.,0.,1.));
#16130=CARTESIAN_POINT('',(10.8511951937867,8.03218294527338,1.));
#16131=CARTESIAN_POINT('Origin',(10.8511951937867,8.03218294527338,4.));
#16132=CARTESIAN_POINT('Origin',(12.0830669365117,6.02195096358128,4.));
#16133=CARTESIAN_POINT('',(12.0830669365117,6.02195096358128,1.));
#16134=CARTESIAN_POINT('',(12.0830669365117,6.02195096358128,1.));
#16135=CARTESIAN_POINT('',(12.0830669365117,6.02195096358128,4.));
#16136=CARTESIAN_POINT('',(12.0830669365117,6.02195096358128,4.));
#16137=CARTESIAN_POINT('',(12.0830669365117,6.02195096358128,4.));
#16138=CARTESIAN_POINT('Origin',(12.7760150883438,6.64438397915208,4.));
#16139=CARTESIAN_POINT('',(11.9741092165742,6.23579252938649,4.));
#16140=CARTESIAN_POINT('',(12.7760150883438,6.64438397915208,4.));
#16141=CARTESIAN_POINT('',(11.9741092165742,6.23579252938649,1.));
#16142=CARTESIAN_POINT('',(11.9741092165742,6.23579252938649,4.));
#16143=CARTESIAN_POINT('',(12.7760150883438,6.64438397915208,1.));
#16144=CARTESIAN_POINT('Origin',(0.,0.,4.));
#16145=CARTESIAN_POINT('',(11.9741092165742,6.23579252938649,4.));
#16146=CARTESIAN_POINT('Origin',(0.,0.,1.));
#16147=CARTESIAN_POINT('',(11.9741092165742,6.23579252938649,1.));
#16148=CARTESIAN_POINT('Origin',(11.9741092165742,6.23579252938649,4.));
#16149=CARTESIAN_POINT('Origin',(12.8763450093096,4.05760264210637,4.));
#16150=CARTESIAN_POINT('',(12.8763450093096,4.05760264210637,1.));
#16151=CARTESIAN_POINT('',(12.8763450093096,4.05760264210637,1.));
#16152=CARTESIAN_POINT('',(12.8763450093096,4.05760264210637,4.));
#16153=CARTESIAN_POINT('',(12.8763450093096,4.05760264210637,4.));
#16154=CARTESIAN_POINT('',(12.8763450093096,4.05760264210637,4.));
#16155=CARTESIAN_POINT('Origin',(13.6581317953252,4.56397150095466,4.));
#16156=CARTESIAN_POINT('',(12.8021809306596,4.28585620601721,4.));
#16157=CARTESIAN_POINT('',(13.6581317953252,4.56397150095466,4.));
#16158=CARTESIAN_POINT('',(12.8021809306596,4.28585620601721,1.));
#16159=CARTESIAN_POINT('',(12.8021809306596,4.28585620601721,4.));
#16160=CARTESIAN_POINT('',(13.6581317953252,4.56397150095466,1.));
#16161=CARTESIAN_POINT('Origin',(0.,0.,4.));
#16162=CARTESIAN_POINT('',(12.8021809306596,4.28585620601721,4.));
#16163=CARTESIAN_POINT('Origin',(0.,0.,1.));
#16164=CARTESIAN_POINT('',(12.8021809306596,4.28585620601721,1.));
#16165=CARTESIAN_POINT('Origin',(12.8021809306596,4.28585620601721,4.));
#16166=CARTESIAN_POINT('',(0.,0.,0.));
#16167=CARTESIAN_POINT('Origin',(-40.,0.,8.));
#16168=CARTESIAN_POINT('',(-36.8,-3.91886975727153E-16,8.));
#16169=CARTESIAN_POINT('Origin',(-40.,0.,8.));
#16170=CARTESIAN_POINT('',(-36.8,-3.91886975727153E-16,0.));
#16171=CARTESIAN_POINT('',(-36.8,-3.91886975727153E-16,8.));
#16172=CARTESIAN_POINT('Origin',(-40.,0.,0.));
#16173=CARTESIAN_POINT('Origin',(0.,0.,8.));
#16174=CARTESIAN_POINT('',(4.2,-5.14351655641888E-16,8.));
#16175=CARTESIAN_POINT('Origin',(0.,0.,8.));
#16176=CARTESIAN_POINT('',(4.2,-5.14351655641888E-16,0.));
#16177=CARTESIAN_POINT('',(4.2,-5.14351655641888E-16,8.));
#16178=CARTESIAN_POINT('Origin',(0.,0.,0.));
#16179=CARTESIAN_POINT('Origin',(0.,0.,8.));
#16180=CARTESIAN_POINT('',(-50.,4.,8.));
#16181=CARTESIAN_POINT('',(-50.,-4.,8.));
#16182=CARTESIAN_POINT('',(-50.,4.,8.));
#16183=CARTESIAN_POINT('',(-45.,-10.,8.));
#16184=CARTESIAN_POINT('',(-50.,-4.,8.));
#16185=CARTESIAN_POINT('',(-40.,-11.,8.));
#16186=CARTESIAN_POINT('',(-45.,-10.,8.));
#16187=CARTESIAN_POINT('',(-8.,-10.,8.));
#16188=CARTESIAN_POINT('',(-40.,-11.,8.));
#16189=CARTESIAN_POINT('',(8.,-10.,8.));
#16190=CARTESIAN_POINT('',(-8.,-10.,8.));
#16191=CARTESIAN_POINT('',(35.,-7.,8.));
#16192=CARTESIAN_POINT('',(8.,-10.,8.));
#16193=CARTESIAN_POINT('',(40.,-3.,8.));
#16194=CARTESIAN_POINT('',(35.,-7.,8.));
#16195=CARTESIAN_POINT('',(40.,3.,8.));
#16196=CARTESIAN_POINT('',(40.,-3.,8.));
#16197=CARTESIAN_POINT('',(35.,7.,8.));
#16198=CARTESIAN_POINT('',(40.,3.,8.));
#16199=CARTESIAN_POINT('',(8.,10.,8.));
#16200=CARTESIAN_POINT('',(35.,7.,8.));
#16201=CARTESIAN_POINT('',(-8.,10.,8.));
#16202=CARTESIAN_POINT('',(8.,10.,8.));
#16203=CARTESIAN_POINT('',(-40.,11.,8.));
#16204=CARTESIAN_POINT('',(-8.,10.,8.));
#16205=CARTESIAN_POINT('',(-45.,10.,8.));
#16206=CARTESIAN_POINT('',(-40.,11.,8.));
#16207=CARTESIAN_POINT('',(-45.,10.,8.));
#16208=CARTESIAN_POINT('Origin',(0.,0.,0.));
#16209=CARTESIAN_POINT('',(-50.,4.,0.));
#16210=CARTESIAN_POINT('',(-50.,-4.,0.));
#16211=CARTESIAN_POINT('',(-50.,4.,0.));
#16212=CARTESIAN_POINT('',(-45.,10.,0.));
#16213=CARTESIAN_POINT('',(-45.,10.,0.));
#16214=CARTESIAN_POINT('',(-40.,11.,0.));
#16215=CARTESIAN_POINT('',(-40.,11.,0.));
#16216=CARTESIAN_POINT('',(-8.,10.,0.));
#16217=CARTESIAN_POINT('',(-8.,10.,0.));
#16218=CARTESIAN_POINT('',(8.,10.,0.));
#16219=CARTESIAN_POINT('',(8.,10.,0.));
#16220=CARTESIAN_POINT('',(35.,7.,0.));
#16221=CARTESIAN_POINT('',(35.,7.,0.));
#16222=CARTESIAN_POINT('',(40.,3.,0.));
#16223=CARTESIAN_POINT('',(40.,3.,0.));
#16224=CARTESIAN_POINT('',(40.,-3.,0.));
#16225=CARTESIAN_POINT('',(40.,-3.,0.));
#16226=CARTESIAN_POINT('',(35.,-7.,0.));
#16227=CARTESIAN_POINT('',(35.,-7.,0.));
#16228=CARTESIAN_POINT('',(8.,-10.,0.));
#16229=CARTESIAN_POINT('',(8.,-10.,0.));
#16230=CARTESIAN_POINT('',(-8.,-10.,0.));
#16231=CARTESIAN_POINT('',(-8.,-10.,0.));
#16232=CARTESIAN_POINT('',(-40.,-11.,0.));
#16233=CARTESIAN_POINT('',(-40.,-11.,0.));
#16234=CARTESIAN_POINT('',(-45.,-10.,0.));
#16235=CARTESIAN_POINT('',(-45.,-10.,0.));
#16236=CARTESIAN_POINT('',(-50.,-4.,0.));
#16237=CARTESIAN_POINT('Origin',(-50.,4.,8.));
#16238=CARTESIAN_POINT('',(-50.,-4.,8.));
#16239=CARTESIAN_POINT('',(-50.,4.,8.));
#16240=CARTESIAN_POINT('Origin',(-50.,-4.,8.));
#16241=CARTESIAN_POINT('',(-45.,-10.,8.));
#16242=CARTESIAN_POINT('Origin',(-45.,-10.,8.));
#16243=CARTESIAN_POINT('',(-40.,-11.,8.));
#16244=CARTESIAN_POINT('Origin',(-40.,-11.,8.));
#16245=CARTESIAN_POINT('',(-8.,-10.,8.));
#16246=CARTESIAN_POINT('Origin',(-8.,-10.,8.));
#16247=CARTESIAN_POINT('',(8.,-10.,8.));
#16248=CARTESIAN_POINT('Origin',(8.,-10.,8.));
#16249=CARTESIAN_POINT('',(35.,-7.,8.));
#16250=CARTESIAN_POINT('Origin',(35.,-7.,8.));
#16251=CARTESIAN_POINT('',(40.,-3.,8.));
#16252=CARTESIAN_POINT('Origin',(40.,-3.,8.));
#16253=CARTESIAN_POINT('',(40.,3.,8.));
#16254=CARTESIAN_POINT('Origin',(40.,3.,8.));
#16255=CARTESIAN_POINT('',(35.,7.,8.));
#16256=CARTESIAN_POINT('Origin',(35.,7.,8.));
#16257=CARTESIAN_POINT('',(8.,10.,8.));
#16258=CARTESIAN_POINT('Origin',(8.,10.,8.));
#16259=CARTESIAN_POINT('',(-8.,10.,8.));
#16260=CARTESIAN_POINT('Origin',(-8.,10.,8.));
#16261=CARTESIAN_POINT('',(-40.,11.,8.));
#16262=CARTESIAN_POINT('Origin',(-40.,11.,8.));
#16263=CARTESIAN_POINT('',(-45.,10.,8.));
#16264=CARTESIAN_POINT('Origin',(-45.,10.,8.));
#16265=CARTESIAN_POINT('',(0.,0.,0.));
#16266=CARTESIAN_POINT('Origin',(0.,0.,65.));
#16267=CARTESIAN_POINT('',(9.,-1.10218211923262E-15,58.));
#16268=CARTESIAN_POINT('Origin',(0.,0.,58.));
#16269=CARTESIAN_POINT('',(7.5,-9.18485099360515E-16,65.));
#16270=CARTESIAN_POINT('',(7.5,-9.18485099360515E-16,65.));
#16271=CARTESIAN_POINT('Origin',(0.,0.,65.));
#16272=CARTESIAN_POINT('Origin',(0.,0.,-5.));
#16273=CARTESIAN_POINT('',(-9.,1.10218211923262E-15,2.));
#16274=CARTESIAN_POINT('',(9.,-1.10218211923262E-15,2.));
#16275=CARTESIAN_POINT('Origin',(0.,0.,2.));
#16276=CARTESIAN_POINT('Origin',(0.,0.,2.));
#16277=CARTESIAN_POINT('',(9.,-1.10218211923262E-15,-5.));
#16278=CARTESIAN_POINT('Origin',(0.,0.,2.));
#16279=CARTESIAN_POINT('',(-8.,-9.79717439317883E-16,-5.55111512312578E-16));
#16280=CARTESIAN_POINT('',(-9.,-1.10218211923262E-15,2.));
#16281=CARTESIAN_POINT('Origin',(0.,0.,0.));
#16282=CARTESIAN_POINT('Origin',(0.,0.,-5.));
#16283=CARTESIAN_POINT('',(3.2,-3.91886975727153E-16,65.));
#16284=CARTESIAN_POINT('Origin',(0.,0.,65.));
#16285=CARTESIAN_POINT('',(3.2,-3.91886975727153E-16,0.));
#16286=CARTESIAN_POINT('',(3.2,-3.91886975727153E-16,-5.));
#16287=CARTESIAN_POINT('Origin',(0.,0.,0.));
#16288=CARTESIAN_POINT('Origin',(3.2,0.,0.));
#16289=CARTESIAN_POINT('Origin',(7.5,0.,65.));
#16290=CARTESIAN_POINT('',(0.,0.,0.));
#16291=CARTESIAN_POINT('Origin',(0.,0.,76.));
#16292=CARTESIAN_POINT('',(5.,-6.12323399573677E-16,73.));
#16293=CARTESIAN_POINT('Origin',(0.,0.,73.));
#16294=CARTESIAN_POINT('',(5.,-6.12323399573677E-16,76.));
#16295=CARTESIAN_POINT('',(5.,-6.12323399573677E-16,76.));
#16296=CARTESIAN_POINT('Origin',(0.,0.,76.));
#16297=CARTESIAN_POINT('Origin',(0.,0.,73.));
#16298=CARTESIAN_POINT('',(3.,-3.67394039744206E-16,0.));
#16299=CARTESIAN_POINT('Origin',(0.,0.,0.));
#16300=CARTESIAN_POINT('',(3.,-3.67394039744206E-16,73.));
#16301=CARTESIAN_POINT('',(3.,-3.67394039744206E-16,73.));
#16302=CARTESIAN_POINT('Origin',(0.,0.,73.));
#16303=CARTESIAN_POINT('Origin',(0.,0.,0.));
#16304=CARTESIAN_POINT('Origin',(0.,0.,76.));
#16305=CARTESIAN_POINT('Origin',(0.,0.,73.));
#16306=CARTESIAN_POINT('',(0.,0.,0.));
#16307=CARTESIAN_POINT('Origin',(0.,0.,6.));
#16308=CARTESIAN_POINT('',(4.2,-5.14351655641888E-16,6.));
#16309=CARTESIAN_POINT('Origin',(0.,0.,6.));
#16310=CARTESIAN_POINT('',(4.2,-5.14351655641888E-16,0.));
#16311=CARTESIAN_POINT('',(4.2,-5.14351655641888E-16,6.));
#16312=CARTESIAN_POINT('Origin',(0.,0.,0.));
#16313=CARTESIAN_POINT('Origin',(0.,0.,6.));
#16314=CARTESIAN_POINT('',(3.75277674973257,-6.5,6.));
#16315=CARTESIAN_POINT('',(7.50555349946513,0.,6.));
#16316=CARTESIAN_POINT('',(3.75277674973257,-6.5,6.));
#16317=CARTESIAN_POINT('',(3.75277674973257,6.5,6.));
#16318=CARTESIAN_POINT('',(7.50555349946513,0.,6.));
#16319=CARTESIAN_POINT('',(-3.75277674973257,6.5,6.));
#16320=CARTESIAN_POINT('',(3.75277674973257,6.5,6.));
#16321=CARTESIAN_POINT('',(-7.50555349946513,9.1916520689492E-16,6.));
#16322=CARTESIAN_POINT('',(-3.75277674973257,6.5,6.));
#16323=CARTESIAN_POINT('',(-3.75277674973257,-6.5,6.));
#16324=CARTESIAN_POINT('',(-7.50555349946513,9.1916520689492E-16,6.));
#16325=CARTESIAN_POINT('',(-3.75277674973257,-6.5,6.));
#16326=CARTESIAN_POINT('Origin',(0.,0.,0.));
#16327=CARTESIAN_POINT('',(3.75277674973257,-6.5,0.));
#16328=CARTESIAN_POINT('',(7.50555349946513,0.,0.));
#16329=CARTESIAN_POINT('',(3.75277674973257,-6.5,0.));
#16330=CARTESIAN_POINT('',(-3.75277674973257,-6.5,0.));
#16331=CARTESIAN_POINT('',(-3.75277674973257,-6.5,0.));
#16332=CARTESIAN_POINT('',(-7.50555349946513,9.1916520689492E-16,0.));
#16333=CARTESIAN_POINT('',(-7.50555349946513,9.1916520689492E-16,0.));
#16334=CARTESIAN_POINT('',(-3.75277674973257,6.5,0.));
#16335=CARTESIAN_POINT('',(-3.75277674973257,6.5,0.));
#16336=CARTESIAN_POINT('',(3.75277674973257,6.5,0.));
#16337=CARTESIAN_POINT('',(3.75277674973257,6.5,0.));
#16338=CARTESIAN_POINT('',(7.50555349946513,0.,0.));
#16339=CARTESIAN_POINT('Origin',(3.75277674973257,-6.5,6.));
#16340=CARTESIAN_POINT('',(7.50555349946513,0.,6.));
#16341=CARTESIAN_POINT('',(3.75277674973257,-6.5,6.));
#16342=CARTESIAN_POINT('Origin',(7.50555349946513,0.,6.));
#16343=CARTESIAN_POINT('',(3.75277674973257,6.5,6.));
#16344=CARTESIAN_POINT('Origin',(3.75277674973257,6.5,6.));
#16345=CARTESIAN_POINT('',(-3.75277674973257,6.5,6.));
#16346=CARTESIAN_POINT('Origin',(-3.75277674973257,6.5,6.));
#16347=CARTESIAN_POINT('',(-7.50555349946513,9.1916520689492E-16,6.));
#16348=CARTESIAN_POINT('Origin',(-7.50555349946513,9.1916520689492E-16,
6.));
#16349=CARTESIAN_POINT('',(-3.75277674973257,-6.5,6.));
#16350=CARTESIAN_POINT('Origin',(-3.75277674973257,-6.5,6.));
#16351=CARTESIAN_POINT('',(0.,0.,0.));
#16352=CARTESIAN_POINT('Origin',(0.,0.,15.));
#16353=CARTESIAN_POINT('',(2.4,-2.93915231795365E-16,3.));
#16354=CARTESIAN_POINT('Origin',(0.,0.,3.));
#16355=CARTESIAN_POINT('',(2.4,-2.93915231795365E-16,15.));
#16356=CARTESIAN_POINT('',(2.4,-2.93915231795365E-16,15.));
#16357=CARTESIAN_POINT('Origin',(0.,0.,15.));
#16358=CARTESIAN_POINT('Origin',(0.,0.,3.));
#16359=CARTESIAN_POINT('',(5.,-6.12323399573677E-16,0.));
#16360=CARTESIAN_POINT('Origin',(0.,0.,0.));
#16361=CARTESIAN_POINT('',(5.,-6.12323399573677E-16,3.));
#16362=CARTESIAN_POINT('',(5.,-6.12323399573677E-16,3.));
#16363=CARTESIAN_POINT('Origin',(0.,0.,3.));
#16364=CARTESIAN_POINT('Origin',(0.,0.,0.));
#16365=CARTESIAN_POINT('',(2.3094010767585,0.,0.));
#16366=CARTESIAN_POINT('',(1.15470053837925,-2.,0.));
#16367=CARTESIAN_POINT('',(1.73205080756888,-1.,0.));
#16368=CARTESIAN_POINT('',(1.15470053837925,2.,0.));
#16369=CARTESIAN_POINT('',(1.73205080756888,1.,0.));
#16370=CARTESIAN_POINT('',(-1.15470053837925,2.,0.));
#16371=CARTESIAN_POINT('',(3.7557864968429E-16,2.,0.));
#16372=CARTESIAN_POINT('',(-2.3094010767585,2.82820063659975E-16,0.));
#16373=CARTESIAN_POINT('',(-1.73205080756888,1.,0.));
#16374=CARTESIAN_POINT('',(-1.15470053837925,-2.,0.));
#16375=CARTESIAN_POINT('',(-1.73205080756888,-1.,0.));
#16376=CARTESIAN_POINT('',(0.,-2.,0.));
#16377=CARTESIAN_POINT('Origin',(0.,0.,3.));
#16378=CARTESIAN_POINT('Origin',(0.,0.,15.));
#16379=CARTESIAN_POINT('Origin',(1.15470053837925,-2.,2.));
#16380=CARTESIAN_POINT('',(1.15470053837925,-2.,2.));
#16381=CARTESIAN_POINT('',(1.15470053837925,-2.,2.));
#16382=CARTESIAN_POINT('',(2.3094010767585,0.,2.));
#16383=CARTESIAN_POINT('',(1.15470053837925,-2.,2.));
#16384=CARTESIAN_POINT('',(2.3094010767585,0.,2.));
#16385=CARTESIAN_POINT('Origin',(2.3094010767585,0.,2.));
#16386=CARTESIAN_POINT('',(1.15470053837925,2.,2.));
#16387=CARTESIAN_POINT('',(2.3094010767585,0.,2.));
#16388=CARTESIAN_POINT('',(1.15470053837925,2.,2.));
#16389=CARTESIAN_POINT('Origin',(1.15470053837925,2.,2.));
#16390=CARTESIAN_POINT('',(-1.15470053837925,2.,2.));
#16391=CARTESIAN_POINT('',(1.15470053837925,2.,2.));
#16392=CARTESIAN_POINT('',(-1.15470053837925,2.,2.));
#16393=CARTESIAN_POINT('Origin',(-1.15470053837925,2.,2.));
#16394=CARTESIAN_POINT('',(-2.3094010767585,2.82820063659975E-16,2.));
#16395=CARTESIAN_POINT('',(-1.15470053837925,2.,2.));
#16396=CARTESIAN_POINT('',(-2.3094010767585,2.82820063659975E-16,2.));
#16397=CARTESIAN_POINT('Origin',(-2.3094010767585,2.82820063659975E-16,
2.));
#16398=CARTESIAN_POINT('',(-1.15470053837925,-2.,2.));
#16399=CARTESIAN_POINT('',(-2.3094010767585,2.82820063659975E-16,2.));
#16400=CARTESIAN_POINT('',(-1.15470053837925,-2.,2.));
#16401=CARTESIAN_POINT('Origin',(-1.15470053837925,-2.,2.));
#16402=CARTESIAN_POINT('',(-1.15470053837925,-2.,2.));
#16403=CARTESIAN_POINT('Origin',(0.,0.,2.));
#16404=CARTESIAN_POINT('',(0.,0.,0.));
#16405=CARTESIAN_POINT('Origin',(0.,0.,16.6));
#16406=CARTESIAN_POINT('',(2.,-2.44929359829471E-16,0.));
#16407=CARTESIAN_POINT('Origin',(0.,0.,0.));
#16408=CARTESIAN_POINT('',(2.,-2.44929359829471E-16,16.6));
#16409=CARTESIAN_POINT('',(2.,-2.44929359829471E-16,16.6));
#16410=CARTESIAN_POINT('Origin',(0.,0.,16.6));
#16411=CARTESIAN_POINT('Origin',(2.3094010767585,-4.,0.));
#16412=CARTESIAN_POINT('',(2.3094010767585,-4.,-4.));
#16413=CARTESIAN_POINT('',(4.61880215351701,0.,-4.));
#16414=CARTESIAN_POINT('',(2.3094010767585,-4.,-4.));
#16415=CARTESIAN_POINT('',(4.61880215351701,0.,0.));
#16416=CARTESIAN_POINT('',(4.61880215351701,0.,0.));
#16417=CARTESIAN_POINT('',(2.3094010767585,-4.,0.));
#16418=CARTESIAN_POINT('',(2.3094010767585,-4.,0.));
#16419=CARTESIAN_POINT('',(2.3094010767585,-4.,0.));
#16420=CARTESIAN_POINT('Origin',(4.61880215351701,0.,0.));
#16421=CARTESIAN_POINT('',(2.3094010767585,4.,-4.));
#16422=CARTESIAN_POINT('',(4.61880215351701,0.,-4.));
#16423=CARTESIAN_POINT('',(2.3094010767585,4.,0.));
#16424=CARTESIAN_POINT('',(2.3094010767585,4.,0.));
#16425=CARTESIAN_POINT('',(4.61880215351701,0.,0.));
#16426=CARTESIAN_POINT('Origin',(2.3094010767585,4.,0.));
#16427=CARTESIAN_POINT('',(-2.3094010767585,4.,-4.));
#16428=CARTESIAN_POINT('',(2.3094010767585,4.,-4.));
#16429=CARTESIAN_POINT('',(-2.3094010767585,4.,0.));
#16430=CARTESIAN_POINT('',(-2.3094010767585,4.,0.));
#16431=CARTESIAN_POINT('',(2.3094010767585,4.,0.));
#16432=CARTESIAN_POINT('Origin',(-2.3094010767585,4.,0.));
#16433=CARTESIAN_POINT('',(-4.61880215351701,5.65640127319951E-16,-4.));
#16434=CARTESIAN_POINT('',(-2.3094010767585,4.,-4.));
#16435=CARTESIAN_POINT('',(-4.61880215351701,5.65640127319951E-16,0.));
#16436=CARTESIAN_POINT('',(-4.61880215351701,5.65640127319951E-16,0.));
#16437=CARTESIAN_POINT('',(-2.3094010767585,4.,0.));
#16438=CARTESIAN_POINT('Origin',(-4.61880215351701,5.65640127319951E-16,
0.));
#16439=CARTESIAN_POINT('',(-2.30940107675851,-4.,-4.));
#16440=CARTESIAN_POINT('',(-4.61880215351701,5.65640127319951E-16,-4.));
#16441=CARTESIAN_POINT('',(-2.30940107675851,-4.,0.));
#16442=CARTESIAN_POINT('',(-2.30940107675851,-4.,0.));
#16443=CARTESIAN_POINT('',(-4.61880215351701,5.65640127319951E-16,0.));
#16444=CARTESIAN_POINT('Origin',(-2.30940107675851,-4.,0.));
#16445=CARTESIAN_POINT('',(-2.30940107675851,-4.,-4.));
#16446=CARTESIAN_POINT('',(-2.30940107675851,-4.,0.));
#16447=CARTESIAN_POINT('Origin',(0.,0.,0.));
#16448=CARTESIAN_POINT('Origin',(0.,0.,-4.));
#16449=CARTESIAN_POINT('Origin',(0.,0.,16.6));
#16450=CARTESIAN_POINT('',(0.,0.,0.));
#16451=CARTESIAN_POINT('Origin',(0.,0.,12.));
#16452=CARTESIAN_POINT('',(1.5,-1.83697019872103E-16,2.));
#16453=CARTESIAN_POINT('Origin',(0.,0.,2.));
#16454=CARTESIAN_POINT('',(1.5,-1.83697019872103E-16,12.));
#16455=CARTESIAN_POINT('',(1.5,-1.83697019872103E-16,12.));
#16456=CARTESIAN_POINT('Origin',(0.,0.,12.));
#16457=CARTESIAN_POINT('Origin',(0.,0.,2.));
#16458=CARTESIAN_POINT('',(3.5,-4.28626379701574E-16,0.));
#16459=CARTESIAN_POINT('Origin',(0.,0.,0.));
#16460=CARTESIAN_POINT('',(3.5,-4.28626379701574E-16,2.));
#16461=CARTESIAN_POINT('',(3.5,-4.28626379701574E-16,2.));
#16462=CARTESIAN_POINT('Origin',(0.,0.,2.));
#16463=CARTESIAN_POINT('Origin',(0.,0.,0.));
#16464=CARTESIAN_POINT('',(1.44337567297406,0.,0.));
#16465=CARTESIAN_POINT('',(0.721687836487032,-1.25,0.));
#16466=CARTESIAN_POINT('',(1.08253175473055,-0.625,0.));
#16467=CARTESIAN_POINT('',(0.721687836487032,1.25,0.));
#16468=CARTESIAN_POINT('',(1.08253175473055,0.625,0.));
#16469=CARTESIAN_POINT('',(-0.721687836487032,1.25,0.));
#16470=CARTESIAN_POINT('',(1.87789324842145E-16,1.25,0.));
#16471=CARTESIAN_POINT('',(-1.44337567297406,1.76762539787484E-16,0.));
#16472=CARTESIAN_POINT('',(-1.08253175473055,0.625,0.));
#16473=CARTESIAN_POINT('',(-0.721687836487033,-1.25,0.));
#16474=CARTESIAN_POINT('',(-1.08253175473055,-0.625,0.));
#16475=CARTESIAN_POINT('',(-1.87789324842145E-16,-1.25,0.));
#16476=CARTESIAN_POINT('Origin',(0.,0.,2.));
#16477=CARTESIAN_POINT('Origin',(0.,0.,12.));
#16478=CARTESIAN_POINT('Origin',(0.721687836487032,-1.25,1.3));
#16479=CARTESIAN_POINT('',(0.721687836487032,-1.25,1.3));
#16480=CARTESIAN_POINT('',(0.721687836487032,-1.25,1.3));
#16481=CARTESIAN_POINT('',(1.44337567297406,0.,1.3));
#16482=CARTESIAN_POINT('',(0.721687836487032,-1.25,1.3));
#16483=CARTESIAN_POINT('',(1.44337567297406,0.,1.3));
#16484=CARTESIAN_POINT('Origin',(1.44337567297406,0.,1.3));
#16485=CARTESIAN_POINT('',(0.721687836487032,1.25,1.3));
#16486=CARTESIAN_POINT('',(1.44337567297406,0.,1.3));
#16487=CARTESIAN_POINT('',(0.721687836487032,1.25,1.3));
#16488=CARTESIAN_POINT('Origin',(0.721687836487032,1.25,1.3));
#16489=CARTESIAN_POINT('',(-0.721687836487032,1.25,1.3));
#16490=CARTESIAN_POINT('',(0.721687836487032,1.25,1.3));
#16491=CARTESIAN_POINT('',(-0.721687836487032,1.25,1.3));
#16492=CARTESIAN_POINT('Origin',(-0.721687836487032,1.25,1.3));
#16493=CARTESIAN_POINT('',(-1.44337567297406,1.76762539787484E-16,1.3));
#16494=CARTESIAN_POINT('',(-0.721687836487032,1.25,1.3));
#16495=CARTESIAN_POINT('',(-1.44337567297406,1.76762539787484E-16,1.3));
#16496=CARTESIAN_POINT('Origin',(-1.44337567297406,1.76762539787484E-16,
1.3));
#16497=CARTESIAN_POINT('',(-0.721687836487033,-1.25,1.3));
#16498=CARTESIAN_POINT('',(-1.44337567297406,1.76762539787484E-16,1.3));
#16499=CARTESIAN_POINT('',(-0.721687836487033,-1.25,1.3));
#16500=CARTESIAN_POINT('Origin',(-0.721687836487033,-1.25,1.3));
#16501=CARTESIAN_POINT('',(-0.721687836487033,-1.25,1.3));
#16502=CARTESIAN_POINT('Origin',(0.,0.,1.3));
#16503=CARTESIAN_POINT('',(0.,0.,0.));
#16504=CARTESIAN_POINT('',(0.,0.,0.));
#16505=CARTESIAN_POINT('',(0.,0.,0.));
#16506=CARTESIAN_POINT('',(0.,0.,0.));
#16507=CARTESIAN_POINT('',(0.,76.,0.));
#16508=CARTESIAN_POINT('',(0.,0.,0.));
#16509=CARTESIAN_POINT('',(0.,0.,0.));
#16510=CARTESIAN_POINT('',(0.,0.,0.));
#16511=CARTESIAN_POINT('',(-124.,0.,21.));
#16512=CARTESIAN_POINT('',(-164.,0.,21.));
#16513=CARTESIAN_POINT('',(0.,144.,55.));
#16514=CARTESIAN_POINT('',(0.,-174.,113.));
#16515=CARTESIAN_POINT('',(0.,0.,0.));
#16516=CARTESIAN_POINT('',(0.,0.,0.));
#16517=CARTESIAN_POINT('',(-150.,0.,21.));
#16518=CARTESIAN_POINT('',(-158.,0.,21.));
#16519=CARTESIAN_POINT('',(-158.,-40.,21.));
#16520=CARTESIAN_POINT('',(0.,-163.,33.));
#16521=CARTESIAN_POINT('',(-150.,-40.,21.));
#16522=CARTESIAN_POINT('',(-164.,0.,21.));
#16523=CARTESIAN_POINT('',(0.,-163.,113.));
#16524=CARTESIAN_POINT('',(-32.,76.,115.8875));
#16525=CARTESIAN_POINT('',(-45.,60.7,26.));
#16526=CARTESIAN_POINT('',(0.,4.99999999999995,72.3));
#16527=CARTESIAN_POINT('',(0.,31.,231.775));
#16528=CARTESIAN_POINT('',(0.,100.,55.));
#16529=CARTESIAN_POINT('',(0.,130.,55.));
#16530=CARTESIAN_POINT('',(0.,138.,55.));
#16531=CARTESIAN_POINT('',(40.,138.,55.));
#16532=CARTESIAN_POINT('',(40.,130.,55.));
#16533=CARTESIAN_POINT('',(0.,144.,55.));
#16534=CARTESIAN_POINT('',(-32.,31.,115.8875));
#16535=CARTESIAN_POINT('',(32.,76.,115.8875));
#16536=CARTESIAN_POINT('',(32.,31.,115.8875));
#16537=CARTESIAN_POINT('',(-127.,-28.,24.));
#16538=CARTESIAN_POINT('',(28.,107.,58.));
#16539=CARTESIAN_POINT('',(-127.,28.,24.));
#16540=CARTESIAN_POINT('',(-28.,107.,58.));
#16541=CARTESIAN_POINT('',(0.,60.7,26.));
#16542=CARTESIAN_POINT('',(45.,60.7,26.));
#16543=CARTESIAN_POINT('',(60.7,-36.,60.));
#16544=CARTESIAN_POINT('',(60.7,0.,60.));
#16545=CARTESIAN_POINT('',(60.7,36.,60.));
#16546=CARTESIAN_POINT('',(0.,17.9999999999999,72.3));
#16547=UNCERTAINTY_MEASURE_WITH_UNIT(LENGTH_MEASURE(0.01),#16599,
'DISTANCE_ACCURACY_VALUE',
'Maximum model space distance between geometric entities at asserted c
onnectivities');
#16548=UNCERTAINTY_MEASURE_WITH_UNIT(LENGTH_MEASURE(0.01),#16599,
'DISTANCE_ACCURACY_VALUE',
'Maximum model space distance between geometric entities at asserted c
onnectivities');
#16549=UNCERTAINTY_MEASURE_WITH_UNIT(LENGTH_MEASURE(0.01),#16599,
'DISTANCE_ACCURACY_VALUE',
'Maximum model space distance between geometric entities at asserted c
onnectivities');
#16550=UNCERTAINTY_MEASURE_WITH_UNIT(LENGTH_MEASURE(0.01),#16599,
'DISTANCE_ACCURACY_VALUE',
'Maximum model space distance between geometric entities at asserted c
onnectivities');
#16551=UNCERTAINTY_MEASURE_WITH_UNIT(LENGTH_MEASURE(0.01),#16599,
'DISTANCE_ACCURACY_VALUE',
'Maximum model space distance between geometric entities at asserted c
onnectivities');
#16552=UNCERTAINTY_MEASURE_WITH_UNIT(LENGTH_MEASURE(0.01),#16599,
'DISTANCE_ACCURACY_VALUE',
'Maximum model space distance between geometric entities at asserted c
onnectivities');
#16553=UNCERTAINTY_MEASURE_WITH_UNIT(LENGTH_MEASURE(0.01),#16599,
'DISTANCE_ACCURACY_VALUE',
'Maximum model space distance between geometric entities at asserted c
onnectivities');
#16554=UNCERTAINTY_MEASURE_WITH_UNIT(LENGTH_MEASURE(0.01),#16599,
'DISTANCE_ACCURACY_VALUE',
'Maximum model space distance between geometric entities at asserted c
onnectivities');
#16555=UNCERTAINTY_MEASURE_WITH_UNIT(LENGTH_MEASURE(0.01),#16599,
'DISTANCE_ACCURACY_VALUE',
'Maximum model space distance between geometric entities at asserted c
onnectivities');
#16556=UNCERTAINTY_MEASURE_WITH_UNIT(LENGTH_MEASURE(0.01),#16599,
'DISTANCE_ACCURACY_VALUE',
'Maximum model space distance between geometric entities at asserted c
onnectivities');
#16557=UNCERTAINTY_MEASURE_WITH_UNIT(LENGTH_MEASURE(0.01),#16599,
'DISTANCE_ACCURACY_VALUE',
'Maximum model space distance between geometric entities at asserted c
onnectivities');
#16558=UNCERTAINTY_MEASURE_WITH_UNIT(LENGTH_MEASURE(0.01),#16599,
'DISTANCE_ACCURACY_VALUE',
'Maximum model space distance between geometric entities at asserted c
onnectivities');
#16559=UNCERTAINTY_MEASURE_WITH_UNIT(LENGTH_MEASURE(0.01),#16599,
'DISTANCE_ACCURACY_VALUE',
'Maximum model space distance between geometric entities at asserted c
onnectivities');
#16560=UNCERTAINTY_MEASURE_WITH_UNIT(LENGTH_MEASURE(0.01),#16599,
'DISTANCE_ACCURACY_VALUE',
'Maximum model space distance between geometric entities at asserted c
onnectivities');
#16561=UNCERTAINTY_MEASURE_WITH_UNIT(LENGTH_MEASURE(0.01),#16599,
'DISTANCE_ACCURACY_VALUE',
'Maximum model space distance between geometric entities at asserted c
onnectivities');
#16562=UNCERTAINTY_MEASURE_WITH_UNIT(LENGTH_MEASURE(0.01),#16599,
'DISTANCE_ACCURACY_VALUE',
'Maximum model space distance between geometric entities at asserted c
onnectivities');
#16563=UNCERTAINTY_MEASURE_WITH_UNIT(LENGTH_MEASURE(0.01),#16599,
'DISTANCE_ACCURACY_VALUE',
'Maximum model space distance between geometric entities at asserted c
onnectivities');
#16564=UNCERTAINTY_MEASURE_WITH_UNIT(LENGTH_MEASURE(0.01),#16599,
'DISTANCE_ACCURACY_VALUE',
'Maximum model space distance between geometric entities at asserted c
onnectivities');
#16565=UNCERTAINTY_MEASURE_WITH_UNIT(LENGTH_MEASURE(0.01),#16599,
'DISTANCE_ACCURACY_VALUE',
'Maximum model space distance between geometric entities at asserted c
onnectivities');
#16566=UNCERTAINTY_MEASURE_WITH_UNIT(LENGTH_MEASURE(0.01),#16599,
'DISTANCE_ACCURACY_VALUE',
'Maximum model space distance between geometric entities at asserted c
onnectivities');
#16567=UNCERTAINTY_MEASURE_WITH_UNIT(LENGTH_MEASURE(0.01),#16599,
'DISTANCE_ACCURACY_VALUE',
'Maximum model space distance between geometric entities at asserted c
onnectivities');
#16568=UNCERTAINTY_MEASURE_WITH_UNIT(LENGTH_MEASURE(0.01),#16599,
'DISTANCE_ACCURACY_VALUE',
'Maximum model space distance between geometric entities at asserted c
onnectivities');
#16569=UNCERTAINTY_MEASURE_WITH_UNIT(LENGTH_MEASURE(0.01),#16599,
'DISTANCE_ACCURACY_VALUE',
'Maximum model space distance between geometric entities at asserted c
onnectivities');
#16570=UNCERTAINTY_MEASURE_WITH_UNIT(LENGTH_MEASURE(0.01),#16599,
'DISTANCE_ACCURACY_VALUE',
'Maximum model space distance between geometric entities at asserted c
onnectivities');
#16571=UNCERTAINTY_MEASURE_WITH_UNIT(LENGTH_MEASURE(0.01),#16599,
'DISTANCE_ACCURACY_VALUE',
'Maximum model space distance between geometric entities at asserted c
onnectivities');
#16572=UNCERTAINTY_MEASURE_WITH_UNIT(LENGTH_MEASURE(0.01),#16599,
'DISTANCE_ACCURACY_VALUE',
'Maximum model space distance between geometric entities at asserted c
onnectivities');
#16573=(
GEOMETRIC_REPRESENTATION_CONTEXT(3)
GLOBAL_UNCERTAINTY_ASSIGNED_CONTEXT((#16547))
GLOBAL_UNIT_ASSIGNED_CONTEXT((#16599,#16601,#16602))
REPRESENTATION_CONTEXT('','3D')
);
#16574=(
GEOMETRIC_REPRESENTATION_CONTEXT(3)
GLOBAL_UNCERTAINTY_ASSIGNED_CONTEXT((#16548))
GLOBAL_UNIT_ASSIGNED_CONTEXT((#16599,#16601,#16602))
REPRESENTATION_CONTEXT('','3D')
);
#16575=(
GEOMETRIC_REPRESENTATION_CONTEXT(3)
GLOBAL_UNCERTAINTY_ASSIGNED_CONTEXT((#16549))
GLOBAL_UNIT_ASSIGNED_CONTEXT((#16599,#16601,#16602))
REPRESENTATION_CONTEXT('','3D')
);
#16576=(
GEOMETRIC_REPRESENTATION_CONTEXT(3)
GLOBAL_UNCERTAINTY_ASSIGNED_CONTEXT((#16550))
GLOBAL_UNIT_ASSIGNED_CONTEXT((#16599,#16601,#16602))
REPRESENTATION_CONTEXT('','3D')
);
#16577=(
GEOMETRIC_REPRESENTATION_CONTEXT(3)
GLOBAL_UNCERTAINTY_ASSIGNED_CONTEXT((#16551))
GLOBAL_UNIT_ASSIGNED_CONTEXT((#16599,#16601,#16602))
REPRESENTATION_CONTEXT('','3D')
);
#16578=(
GEOMETRIC_REPRESENTATION_CONTEXT(3)
GLOBAL_UNCERTAINTY_ASSIGNED_CONTEXT((#16552))
GLOBAL_UNIT_ASSIGNED_CONTEXT((#16599,#16601,#16602))
REPRESENTATION_CONTEXT('','3D')
);
#16579=(
GEOMETRIC_REPRESENTATION_CONTEXT(3)
GLOBAL_UNCERTAINTY_ASSIGNED_CONTEXT((#16553))
GLOBAL_UNIT_ASSIGNED_CONTEXT((#16599,#16601,#16602))
REPRESENTATION_CONTEXT('','3D')
);
#16580=(
GEOMETRIC_REPRESENTATION_CONTEXT(3)
GLOBAL_UNCERTAINTY_ASSIGNED_CONTEXT((#16554))
GLOBAL_UNIT_ASSIGNED_CONTEXT((#16599,#16601,#16602))
REPRESENTATION_CONTEXT('','3D')
);
#16581=(
GEOMETRIC_REPRESENTATION_CONTEXT(3)
GLOBAL_UNCERTAINTY_ASSIGNED_CONTEXT((#16555))
GLOBAL_UNIT_ASSIGNED_CONTEXT((#16599,#16601,#16602))
REPRESENTATION_CONTEXT('','3D')
);
#16582=(
GEOMETRIC_REPRESENTATION_CONTEXT(3)
GLOBAL_UNCERTAINTY_ASSIGNED_CONTEXT((#16556))
GLOBAL_UNIT_ASSIGNED_CONTEXT((#16599,#16601,#16602))
REPRESENTATION_CONTEXT('','3D')
);
#16583=(
GEOMETRIC_REPRESENTATION_CONTEXT(3)
GLOBAL_UNCERTAINTY_ASSIGNED_CONTEXT((#16557))
GLOBAL_UNIT_ASSIGNED_CONTEXT((#16599,#16601,#16602))
REPRESENTATION_CONTEXT('','3D')
);
#16584=(
GEOMETRIC_REPRESENTATION_CONTEXT(3)
GLOBAL_UNCERTAINTY_ASSIGNED_CONTEXT((#16558))
GLOBAL_UNIT_ASSIGNED_CONTEXT((#16599,#16601,#16602))
REPRESENTATION_CONTEXT('','3D')
);
#16585=(
GEOMETRIC_REPRESENTATION_CONTEXT(3)
GLOBAL_UNCERTAINTY_ASSIGNED_CONTEXT((#16559))
GLOBAL_UNIT_ASSIGNED_CONTEXT((#16599,#16601,#16602))
REPRESENTATION_CONTEXT('','3D')
);
#16586=(
GEOMETRIC_REPRESENTATION_CONTEXT(3)
GLOBAL_UNCERTAINTY_ASSIGNED_CONTEXT((#16560))
GLOBAL_UNIT_ASSIGNED_CONTEXT((#16599,#16601,#16602))
REPRESENTATION_CONTEXT('','3D')
);
#16587=(
GEOMETRIC_REPRESENTATION_CONTEXT(3)
GLOBAL_UNCERTAINTY_ASSIGNED_CONTEXT((#16561))
GLOBAL_UNIT_ASSIGNED_CONTEXT((#16599,#16601,#16602))
REPRESENTATION_CONTEXT('','3D')
);
#16588=(
GEOMETRIC_REPRESENTATION_CONTEXT(3)
GLOBAL_UNCERTAINTY_ASSIGNED_CONTEXT((#16562))
GLOBAL_UNIT_ASSIGNED_CONTEXT((#16599,#16601,#16602))
REPRESENTATION_CONTEXT('','3D')
);
#16589=(
GEOMETRIC_REPRESENTATION_CONTEXT(3)
GLOBAL_UNCERTAINTY_ASSIGNED_CONTEXT((#16563))
GLOBAL_UNIT_ASSIGNED_CONTEXT((#16599,#16601,#16602))
REPRESENTATION_CONTEXT('','3D')
);
#16590=(
GEOMETRIC_REPRESENTATION_CONTEXT(3)
GLOBAL_UNCERTAINTY_ASSIGNED_CONTEXT((#16564))
GLOBAL_UNIT_ASSIGNED_CONTEXT((#16599,#16601,#16602))
REPRESENTATION_CONTEXT('','3D')
);
#16591=(
GEOMETRIC_REPRESENTATION_CONTEXT(3)
GLOBAL_UNCERTAINTY_ASSIGNED_CONTEXT((#16565))
GLOBAL_UNIT_ASSIGNED_CONTEXT((#16599,#16601,#16602))
REPRESENTATION_CONTEXT('','3D')
);
#16592=(
GEOMETRIC_REPRESENTATION_CONTEXT(3)
GLOBAL_UNCERTAINTY_ASSIGNED_CONTEXT((#16566))
GLOBAL_UNIT_ASSIGNED_CONTEXT((#16599,#16601,#16602))
REPRESENTATION_CONTEXT('','3D')
);
#16593=(
GEOMETRIC_REPRESENTATION_CONTEXT(3)
GLOBAL_UNCERTAINTY_ASSIGNED_CONTEXT((#16567))
GLOBAL_UNIT_ASSIGNED_CONTEXT((#16599,#16601,#16602))
REPRESENTATION_CONTEXT('','3D')
);
#16594=(
GEOMETRIC_REPRESENTATION_CONTEXT(3)
GLOBAL_UNCERTAINTY_ASSIGNED_CONTEXT((#16568))
GLOBAL_UNIT_ASSIGNED_CONTEXT((#16599,#16601,#16602))
REPRESENTATION_CONTEXT('','3D')
);
#16595=(
GEOMETRIC_REPRESENTATION_CONTEXT(3)
GLOBAL_UNCERTAINTY_ASSIGNED_CONTEXT((#16569))
GLOBAL_UNIT_ASSIGNED_CONTEXT((#16599,#16601,#16602))
REPRESENTATION_CONTEXT('','3D')
);
#16596=(
GEOMETRIC_REPRESENTATION_CONTEXT(3)
GLOBAL_UNCERTAINTY_ASSIGNED_CONTEXT((#16570))
GLOBAL_UNIT_ASSIGNED_CONTEXT((#16599,#16601,#16602))
REPRESENTATION_CONTEXT('','3D')
);
#16597=(
GEOMETRIC_REPRESENTATION_CONTEXT(3)
GLOBAL_UNCERTAINTY_ASSIGNED_CONTEXT((#16571))
GLOBAL_UNIT_ASSIGNED_CONTEXT((#16599,#16601,#16602))
REPRESENTATION_CONTEXT('','3D')
);
#16598=(
GEOMETRIC_REPRESENTATION_CONTEXT(3)
GLOBAL_UNCERTAINTY_ASSIGNED_CONTEXT((#16572))
GLOBAL_UNIT_ASSIGNED_CONTEXT((#16599,#16601,#16602))
REPRESENTATION_CONTEXT('','3D')
);
#16599=(
LENGTH_UNIT()
NAMED_UNIT(*)
SI_UNIT(.MILLI.,.METRE.)
);
#16600=(
LENGTH_UNIT()
NAMED_UNIT(*)
SI_UNIT($,.METRE.)
);
#16601=(
NAMED_UNIT(*)
PLANE_ANGLE_UNIT()
SI_UNIT($,.RADIAN.)
);
#16602=(
NAMED_UNIT(*)
SI_UNIT($,.STERADIAN.)
SOLID_ANGLE_UNIT()
);
#16603=SHAPE_DEFINITION_REPRESENTATION(#16628,#16697);
#16604=SHAPE_DEFINITION_REPRESENTATION(#16629,#16698);
#16605=SHAPE_DEFINITION_REPRESENTATION(#16630,#16699);
#16606=SHAPE_DEFINITION_REPRESENTATION(#16631,#16700);
#16607=SHAPE_DEFINITION_REPRESENTATION(#16632,#16701);
#16608=SHAPE_DEFINITION_REPRESENTATION(#16633,#16702);
#16609=SHAPE_DEFINITION_REPRESENTATION(#16634,#16703);
#16610=SHAPE_DEFINITION_REPRESENTATION(#16635,#16704);
#16611=SHAPE_DEFINITION_REPRESENTATION(#16636,#16705);
#16612=SHAPE_DEFINITION_REPRESENTATION(#16637,#16706);
#16613=SHAPE_DEFINITION_REPRESENTATION(#16638,#16707);
#16614=SHAPE_DEFINITION_REPRESENTATION(#16639,#16708);
#16615=SHAPE_DEFINITION_REPRESENTATION(#16640,#16709);
#16616=SHAPE_DEFINITION_REPRESENTATION(#16641,#16710);
#16617=SHAPE_DEFINITION_REPRESENTATION(#16642,#16711);
#16618=SHAPE_DEFINITION_REPRESENTATION(#16643,#16712);
#16619=SHAPE_DEFINITION_REPRESENTATION(#16644,#16713);
#16620=SHAPE_DEFINITION_REPRESENTATION(#16645,#16714);
#16621=SHAPE_DEFINITION_REPRESENTATION(#16646,#16715);
#16622=SHAPE_DEFINITION_REPRESENTATION(#16647,#16716);
#16623=SHAPE_DEFINITION_REPRESENTATION(#16648,#16717);
#16624=SHAPE_DEFINITION_REPRESENTATION(#16649,#16718);
#16625=SHAPE_DEFINITION_REPRESENTATION(#16650,#16719);
#16626=SHAPE_DEFINITION_REPRESENTATION(#16651,#16720);
#16627=SHAPE_DEFINITION_REPRESENTATION(#16652,#16721);
#16628=PRODUCT_DEFINITION_SHAPE('',$,#16723);
#16629=PRODUCT_DEFINITION_SHAPE('',$,#16724);
#16630=PRODUCT_DEFINITION_SHAPE('',$,#16725);
#16631=PRODUCT_DEFINITION_SHAPE('',$,#16726);
#16632=PRODUCT_DEFINITION_SHAPE('',$,#16727);
#16633=PRODUCT_DEFINITION_SHAPE('',$,#16728);
#16634=PRODUCT_DEFINITION_SHAPE('',$,#16729);
#16635=PRODUCT_DEFINITION_SHAPE('',$,#16730);
#16636=PRODUCT_DEFINITION_SHAPE('',$,#16731);
#16637=PRODUCT_DEFINITION_SHAPE('',$,#16732);
#16638=PRODUCT_DEFINITION_SHAPE('',$,#16733);
#16639=PRODUCT_DEFINITION_SHAPE('',$,#16734);
#16640=PRODUCT_DEFINITION_SHAPE('',$,#16735);
#16641=PRODUCT_DEFINITION_SHAPE('',$,#16736);
#16642=PRODUCT_DEFINITION_SHAPE('',$,#16737);
#16643=PRODUCT_DEFINITION_SHAPE('',$,#16738);
#16644=PRODUCT_DEFINITION_SHAPE('',$,#16739);
#16645=PRODUCT_DEFINITION_SHAPE('',$,#16740);
#16646=PRODUCT_DEFINITION_SHAPE('',$,#16741);
#16647=PRODUCT_DEFINITION_SHAPE('',$,#16742);
#16648=PRODUCT_DEFINITION_SHAPE('',$,#16743);
#16649=PRODUCT_DEFINITION_SHAPE('',$,#16744);
#16650=PRODUCT_DEFINITION_SHAPE('',$,#16745);
#16651=PRODUCT_DEFINITION_SHAPE('',$,#16746);
#16652=PRODUCT_DEFINITION_SHAPE('',$,#16747);
#16653=PRODUCT_DEFINITION_SHAPE($,$,#143);
#16654=PRODUCT_DEFINITION_SHAPE($,$,#144);
#16655=PRODUCT_DEFINITION_SHAPE($,$,#145);
#16656=PRODUCT_DEFINITION_SHAPE($,$,#146);
#16657=PRODUCT_DEFINITION_SHAPE($,$,#147);
#16658=PRODUCT_DEFINITION_SHAPE($,$,#148);
#16659=PRODUCT_DEFINITION_SHAPE($,$,#149);
#16660=PRODUCT_DEFINITION_SHAPE($,$,#150);
#16661=PRODUCT_DEFINITION_SHAPE($,$,#151);
#16662=PRODUCT_DEFINITION_SHAPE($,$,#152);
#16663=PRODUCT_DEFINITION_SHAPE($,$,#153);
#16664=PRODUCT_DEFINITION_SHAPE($,$,#154);
#16665=PRODUCT_DEFINITION_SHAPE($,$,#155);
#16666=PRODUCT_DEFINITION_SHAPE($,$,#156);
#16667=PRODUCT_DEFINITION_SHAPE($,$,#157);
#16668=PRODUCT_DEFINITION_SHAPE($,$,#158);
#16669=PRODUCT_DEFINITION_SHAPE($,$,#159);
#16670=PRODUCT_DEFINITION_SHAPE($,$,#160);
#16671=PRODUCT_DEFINITION_SHAPE($,$,#161);
#16672=PRODUCT_DEFINITION_SHAPE($,$,#162);
#16673=PRODUCT_DEFINITION_SHAPE($,$,#163);
#16674=PRODUCT_DEFINITION_SHAPE($,$,#164);
#16675=PRODUCT_DEFINITION_SHAPE($,$,#165);
#16676=PRODUCT_DEFINITION_SHAPE($,$,#166);
#16677=PRODUCT_DEFINITION_SHAPE($,$,#167);
#16678=PRODUCT_DEFINITION_SHAPE($,$,#168);
#16679=PRODUCT_DEFINITION_SHAPE($,$,#169);
#16680=PRODUCT_DEFINITION_SHAPE($,$,#170);
#16681=PRODUCT_DEFINITION_SHAPE($,$,#171);
#16682=PRODUCT_DEFINITION_SHAPE($,$,#172);
#16683=PRODUCT_DEFINITION_SHAPE($,$,#173);
#16684=PRODUCT_DEFINITION_SHAPE($,$,#174);
#16685=PRODUCT_DEFINITION_SHAPE($,$,#175);
#16686=PRODUCT_DEFINITION_SHAPE($,$,#176);
#16687=PRODUCT_DEFINITION_SHAPE($,$,#177);
#16688=PRODUCT_DEFINITION_SHAPE($,$,#178);
#16689=PRODUCT_DEFINITION_SHAPE($,$,#179);
#16690=PRODUCT_DEFINITION_SHAPE($,$,#180);
#16691=PRODUCT_DEFINITION_SHAPE($,$,#181);
#16692=PRODUCT_DEFINITION_SHAPE($,$,#182);
#16693=PRODUCT_DEFINITION_SHAPE($,$,#183);
#16694=PRODUCT_DEFINITION_SHAPE($,$,#184);
#16695=PRODUCT_DEFINITION_SHAPE($,$,#185);
#16696=PRODUCT_DEFINITION_SHAPE($,$,#186);
#16697=SHAPE_REPRESENTATION('',(#10076,#10884,#10885,#10886,#10887,#10888,
#10889,#10890,#10891,#10892,#10893,#10894,#10895,#10896,#10897,#10898,#10899,
#10900,#10901,#10902,#10903,#10904,#10905,#10906,#10907,#10908,#10909,#10910,
#10911,#10912,#10913,#10914,#10915,#10916,#10917,#10918,#10919,#10920,#10921,
#10922,#10923,#10924,#10925,#10926,#10927),#16573);
#16698=SHAPE_REPRESENTATION('',(#10077),#16574);
#16699=SHAPE_REPRESENTATION('',(#10132),#16575);
#16700=SHAPE_REPRESENTATION('',(#10189),#16576);
#16701=SHAPE_REPRESENTATION('',(#10266),#16577);
#16702=SHAPE_REPRESENTATION('',(#10299),#16578);
#16703=SHAPE_REPRESENTATION('',(#10306),#16579);
#16704=SHAPE_REPRESENTATION('',(#10313),#16580);
#16705=SHAPE_REPRESENTATION('',(#10334),#16581);
#16706=SHAPE_REPRESENTATION('',(#10356),#16582);
#16707=SHAPE_REPRESENTATION('',(#10378),#16583);
#16708=SHAPE_REPRESENTATION('',(#10404),#16584);
#16709=SHAPE_REPRESENTATION('',(#10414),#16585);
#16710=SHAPE_REPRESENTATION('',(#10424),#16586);
#16711=SHAPE_REPRESENTATION('',(#10440),#16587);
#16712=SHAPE_REPRESENTATION('',(#10446),#16588);
#16713=SHAPE_REPRESENTATION('',(#10467),#16589);
#16714=SHAPE_REPRESENTATION('',(#10487),#16590);
#16715=SHAPE_REPRESENTATION('',(#10778),#16591);
#16716=SHAPE_REPRESENTATION('',(#10801),#16592);
#16717=SHAPE_REPRESENTATION('',(#10815),#16593);
#16718=SHAPE_REPRESENTATION('',(#10825),#16594);
#16719=SHAPE_REPRESENTATION('',(#10837),#16595);
#16720=SHAPE_REPRESENTATION('',(#10854),#16596);
#16721=SHAPE_REPRESENTATION('',(#10867),#16597);
#16722=PRODUCT_DEFINITION_CONTEXT('part definition',#16799,'design');
#16723=PRODUCT_DEFINITION('assembly','TAS-017',#16748,#16722);
#16724=PRODUCT_DEFINITION('P01_Mounting_Base','P01_Mounting_Base',#16749,
#16722);
#16725=PRODUCT_DEFINITION('P02_Cross_Slide_Saddle',
'P02_Cross_Slide_Saddle',#16750,#16722);
#16726=PRODUCT_DEFINITION('P03_Upper_Vise_Body','P03_Upper_Vise_Body',#16751,
#16722);
#16727=PRODUCT_DEFINITION('P04_Moving_Jaw','P04_Moving_Jaw',#16752,#16722);
#16728=PRODUCT_DEFINITION('P06_Lower_Axis_Gib','P06_Lower_Axis_Gib',#16753,
#16722);
#16729=PRODUCT_DEFINITION('P07_Upper_Axis_Gib','P07_Upper_Axis_Gib',#16754,
#16722);
#16730=PRODUCT_DEFINITION('P08_Jaw_Retainer_Bar','P08_Jaw_Retainer_Bar',
#16755,#16722);
#16731=PRODUCT_DEFINITION('P10_Lower_Feed_Screw','P10_Lower_Feed_Screw',
#16756,#16722);
#16732=PRODUCT_DEFINITION('P11_Upper_Feed_Screw','P11_Upper_Feed_Screw',
#16757,#16722);
#16733=PRODUCT_DEFINITION('P12_Jaw_Clamping_Screw',
'P12_Jaw_Clamping_Screw',#16758,#16722);
#16734=PRODUCT_DEFINITION('P13_Lower_Feed_Nut','P13_Lower_Feed_Nut',#16759,
#16722);
#16735=PRODUCT_DEFINITION('P14_Upper_Feed_Nut','P14_Upper_Feed_Nut',#16760,
#16722);
#16736=PRODUCT_DEFINITION('P18_Folding_Jaw_Handle',
'P18_Folding_Jaw_Handle',#16761,#16722);
#16737=PRODUCT_DEFINITION('F05_Handle_Pivot_Pin','F05_Handle_Pivot_Pin',
#16762,#16722);
#16738=PRODUCT_DEFINITION('P05_Replaceable_Jaw_Plate',
'P05_Replaceable_Jaw_Plate',#16763,#16722);
#16739=PRODUCT_DEFINITION('P09_Feed_Bearing_Bracket',
'P09_Feed_Bearing_Bracket',#16764,#16722);
#16740=PRODUCT_DEFINITION('P15_Graduated_Feed_Dial',
'P15_Graduated_Feed_Dial',#16765,#16722);
#16741=PRODUCT_DEFINITION('P16_Cross_Feed_Crank','P16_Cross_Feed_Crank',
#16766,#16722);
#16742=PRODUCT_DEFINITION('P17_Revolving_Hand_Grip',
'P17_Revolving_Hand_Grip',#16767,#16722);
#16743=PRODUCT_DEFINITION('F01_Grip_Shoulder_Axle',
'F01_Grip_Shoulder_Axle',#16768,#16722);
#16744=PRODUCT_DEFINITION('F02_M8_Crank_Retaining_Nut',
'F02_M8_Crank_Retaining_Nut',#16769,#16722);
#16745=PRODUCT_DEFINITION('F03_M6x12_Low_Head_Screw',
'F03_M6x12_Low_Head_Screw',#16770,#16722);
#16746=PRODUCT_DEFINITION('F04_M5_Gib_Adjusting_Screw',
'F04_M5_Gib_Adjusting_Screw',#16771,#16722);
#16747=PRODUCT_DEFINITION('F06_M4x10_Retainer_Screw',
'F06_M4x10_Retainer_Screw',#16772,#16722);
#16748=PRODUCT_DEFINITION_FORMATION('',$,#16801);
#16749=PRODUCT_DEFINITION_FORMATION('',$,#16802);
#16750=PRODUCT_DEFINITION_FORMATION('',$,#16803);
#16751=PRODUCT_DEFINITION_FORMATION('',$,#16804);
#16752=PRODUCT_DEFINITION_FORMATION('',$,#16805);
#16753=PRODUCT_DEFINITION_FORMATION('',$,#16806);
#16754=PRODUCT_DEFINITION_FORMATION('',$,#16807);
#16755=PRODUCT_DEFINITION_FORMATION('',$,#16808);
#16756=PRODUCT_DEFINITION_FORMATION('',$,#16809);
#16757=PRODUCT_DEFINITION_FORMATION('',$,#16810);
#16758=PRODUCT_DEFINITION_FORMATION('',$,#16811);
#16759=PRODUCT_DEFINITION_FORMATION('',$,#16812);
#16760=PRODUCT_DEFINITION_FORMATION('',$,#16813);
#16761=PRODUCT_DEFINITION_FORMATION('',$,#16814);
#16762=PRODUCT_DEFINITION_FORMATION('',$,#16815);
#16763=PRODUCT_DEFINITION_FORMATION('',$,#16816);
#16764=PRODUCT_DEFINITION_FORMATION('',$,#16817);
#16765=PRODUCT_DEFINITION_FORMATION('',$,#16818);
#16766=PRODUCT_DEFINITION_FORMATION('',$,#16819);
#16767=PRODUCT_DEFINITION_FORMATION('',$,#16820);
#16768=PRODUCT_DEFINITION_FORMATION('',$,#16821);
#16769=PRODUCT_DEFINITION_FORMATION('',$,#16822);
#16770=PRODUCT_DEFINITION_FORMATION('',$,#16823);
#16771=PRODUCT_DEFINITION_FORMATION('',$,#16824);
#16772=PRODUCT_DEFINITION_FORMATION('',$,#16825);
#16773=PRODUCT_RELATED_PRODUCT_CATEGORY('TAS-017','TAS-017',(#16801));
#16774=PRODUCT_RELATED_PRODUCT_CATEGORY('P01_Mounting_Base',
'P01_Mounting_Base',(#16802));
#16775=PRODUCT_RELATED_PRODUCT_CATEGORY('P02_Cross_Slide_Saddle',
'P02_Cross_Slide_Saddle',(#16803));
#16776=PRODUCT_RELATED_PRODUCT_CATEGORY('P03_Upper_Vise_Body',
'P03_Upper_Vise_Body',(#16804));
#16777=PRODUCT_RELATED_PRODUCT_CATEGORY('P04_Moving_Jaw',
'P04_Moving_Jaw',(#16805));
#16778=PRODUCT_RELATED_PRODUCT_CATEGORY('P06_Lower_Axis_Gib',
'P06_Lower_Axis_Gib',(#16806));
#16779=PRODUCT_RELATED_PRODUCT_CATEGORY('P07_Upper_Axis_Gib',
'P07_Upper_Axis_Gib',(#16807));
#16780=PRODUCT_RELATED_PRODUCT_CATEGORY('P08_Jaw_Retainer_Bar',
'P08_Jaw_Retainer_Bar',(#16808));
#16781=PRODUCT_RELATED_PRODUCT_CATEGORY('P10_Lower_Feed_Screw',
'P10_Lower_Feed_Screw',(#16809));
#16782=PRODUCT_RELATED_PRODUCT_CATEGORY('P11_Upper_Feed_Screw',
'P11_Upper_Feed_Screw',(#16810));
#16783=PRODUCT_RELATED_PRODUCT_CATEGORY('P12_Jaw_Clamping_Screw',
'P12_Jaw_Clamping_Screw',(#16811));
#16784=PRODUCT_RELATED_PRODUCT_CATEGORY('P13_Lower_Feed_Nut',
'P13_Lower_Feed_Nut',(#16812));
#16785=PRODUCT_RELATED_PRODUCT_CATEGORY('P14_Upper_Feed_Nut',
'P14_Upper_Feed_Nut',(#16813));
#16786=PRODUCT_RELATED_PRODUCT_CATEGORY('P18_Folding_Jaw_Handle',
'P18_Folding_Jaw_Handle',(#16814));
#16787=PRODUCT_RELATED_PRODUCT_CATEGORY('F05_Handle_Pivot_Pin',
'F05_Handle_Pivot_Pin',(#16815));
#16788=PRODUCT_RELATED_PRODUCT_CATEGORY('P05_Replaceable_Jaw_Plate',
'P05_Replaceable_Jaw_Plate',(#16816));
#16789=PRODUCT_RELATED_PRODUCT_CATEGORY('P09_Feed_Bearing_Bracket',
'P09_Feed_Bearing_Bracket',(#16817));
#16790=PRODUCT_RELATED_PRODUCT_CATEGORY('P15_Graduated_Feed_Dial',
'P15_Graduated_Feed_Dial',(#16818));
#16791=PRODUCT_RELATED_PRODUCT_CATEGORY('P16_Cross_Feed_Crank',
'P16_Cross_Feed_Crank',(#16819));
#16792=PRODUCT_RELATED_PRODUCT_CATEGORY('P17_Revolving_Hand_Grip',
'P17_Revolving_Hand_Grip',(#16820));
#16793=PRODUCT_RELATED_PRODUCT_CATEGORY('F01_Grip_Shoulder_Axle',
'F01_Grip_Shoulder_Axle',(#16821));
#16794=PRODUCT_RELATED_PRODUCT_CATEGORY('F02_M8_Crank_Retaining_Nut',
'F02_M8_Crank_Retaining_Nut',(#16822));
#16795=PRODUCT_RELATED_PRODUCT_CATEGORY('F03_M6x12_Low_Head_Screw',
'F03_M6x12_Low_Head_Screw',(#16823));
#16796=PRODUCT_RELATED_PRODUCT_CATEGORY('F04_M5_Gib_Adjusting_Screw',
'F04_M5_Gib_Adjusting_Screw',(#16824));
#16797=PRODUCT_RELATED_PRODUCT_CATEGORY('F06_M4x10_Retainer_Screw',
'F06_M4x10_Retainer_Screw',(#16825));
#16798=APPLICATION_PROTOCOL_DEFINITION('international standard',
'automotive_design',2009,#16799);
#16799=APPLICATION_CONTEXT(
'Core Data for Automotive Mechanical Design Process');
#16800=PRODUCT_CONTEXT('part definition',#16799,'mechanical');
#16801=PRODUCT('assembly','TAS-017','STEP AP203',(#16800));
#16802=PRODUCT('P01_Mounting_Base','P01_Mounting_Base',$,(#16800));
#16803=PRODUCT('P02_Cross_Slide_Saddle','P02_Cross_Slide_Saddle',$,(#16800));
#16804=PRODUCT('P03_Upper_Vise_Body','P03_Upper_Vise_Body',$,(#16800));
#16805=PRODUCT('P04_Moving_Jaw','P04_Moving_Jaw',$,(#16800));
#16806=PRODUCT('P06_Lower_Axis_Gib','P06_Lower_Axis_Gib',$,(#16800));
#16807=PRODUCT('P07_Upper_Axis_Gib','P07_Upper_Axis_Gib',$,(#16800));
#16808=PRODUCT('P08_Jaw_Retainer_Bar','P08_Jaw_Retainer_Bar',$,(#16800));
#16809=PRODUCT('P10_Lower_Feed_Screw','P10_Lower_Feed_Screw',$,(#16800));
#16810=PRODUCT('P11_Upper_Feed_Screw','P11_Upper_Feed_Screw',$,(#16800));
#16811=PRODUCT('P12_Jaw_Clamping_Screw','P12_Jaw_Clamping_Screw',$,(#16800));
#16812=PRODUCT('P13_Lower_Feed_Nut','P13_Lower_Feed_Nut',$,(#16800));
#16813=PRODUCT('P14_Upper_Feed_Nut','P14_Upper_Feed_Nut',$,(#16800));
#16814=PRODUCT('P18_Folding_Jaw_Handle','P18_Folding_Jaw_Handle',$,(#16800));
#16815=PRODUCT('F05_Handle_Pivot_Pin','F05_Handle_Pivot_Pin',$,(#16800));
#16816=PRODUCT('P05_Replaceable_Jaw_Plate','P05_Replaceable_Jaw_Plate',
$,(#16800));
#16817=PRODUCT('P09_Feed_Bearing_Bracket','P09_Feed_Bearing_Bracket',$,
(#16800));
#16818=PRODUCT('P15_Graduated_Feed_Dial','P15_Graduated_Feed_Dial',$,(#16800));
#16819=PRODUCT('P16_Cross_Feed_Crank','P16_Cross_Feed_Crank',$,(#16800));
#16820=PRODUCT('P17_Revolving_Hand_Grip','P17_Revolving_Hand_Grip',$,(#16800));
#16821=PRODUCT('F01_Grip_Shoulder_Axle','F01_Grip_Shoulder_Axle',$,(#16800));
#16822=PRODUCT('F02_M8_Crank_Retaining_Nut',
'F02_M8_Crank_Retaining_Nut',$,(#16800));
#16823=PRODUCT('F03_M6x12_Low_Head_Screw','F03_M6x12_Low_Head_Screw',$,
(#16800));
#16824=PRODUCT('F04_M5_Gib_Adjusting_Screw',
'F04_M5_Gib_Adjusting_Screw',$,(#16800));
#16825=PRODUCT('F06_M4x10_Retainer_Screw','F06_M4x10_Retainer_Screw',$,
(#16800));
#16826=PRESENTATION_STYLE_ASSIGNMENT((#16835));
#16827=PRESENTATION_STYLE_ASSIGNMENT((#16836));
#16828=PRESENTATION_STYLE_ASSIGNMENT((#16837));
#16829=PRESENTATION_STYLE_ASSIGNMENT((#16838));
#16830=PRESENTATION_STYLE_ASSIGNMENT((#16839));
#16831=PRESENTATION_STYLE_ASSIGNMENT((#16840));
#16832=PRESENTATION_STYLE_ASSIGNMENT((#16841));
#16833=PRESENTATION_STYLE_ASSIGNMENT((#16842));
#16834=PRESENTATION_STYLE_ASSIGNMENT((#16843));
#16835=SURFACE_STYLE_USAGE(.BOTH.,#16844);
#16836=SURFACE_STYLE_USAGE(.BOTH.,#16845);
#16837=SURFACE_STYLE_USAGE(.BOTH.,#16846);
#16838=SURFACE_STYLE_USAGE(.BOTH.,#16847);
#16839=SURFACE_STYLE_USAGE(.BOTH.,#16848);
#16840=SURFACE_STYLE_USAGE(.BOTH.,#16849);
#16841=SURFACE_STYLE_USAGE(.BOTH.,#16850);
#16842=SURFACE_STYLE_USAGE(.BOTH.,#16851);
#16843=SURFACE_STYLE_USAGE(.BOTH.,#16852);
#16844=SURFACE_SIDE_STYLE('',(#16853));
#16845=SURFACE_SIDE_STYLE('',(#16854));
#16846=SURFACE_SIDE_STYLE('',(#16855));
#16847=SURFACE_SIDE_STYLE('',(#16856));
#16848=SURFACE_SIDE_STYLE('',(#16857));
#16849=SURFACE_SIDE_STYLE('',(#16858));
#16850=SURFACE_SIDE_STYLE('',(#16859));
#16851=SURFACE_SIDE_STYLE('',(#16860));
#16852=SURFACE_SIDE_STYLE('',(#16861));
#16853=SURFACE_STYLE_FILL_AREA(#16862);
#16854=SURFACE_STYLE_FILL_AREA(#16863);
#16855=SURFACE_STYLE_FILL_AREA(#16864);
#16856=SURFACE_STYLE_FILL_AREA(#16865);
#16857=SURFACE_STYLE_FILL_AREA(#16866);
#16858=SURFACE_STYLE_FILL_AREA(#16867);
#16859=SURFACE_STYLE_FILL_AREA(#16868);
#16860=SURFACE_STYLE_FILL_AREA(#16869);
#16861=SURFACE_STYLE_FILL_AREA(#16870);
#16862=FILL_AREA_STYLE('Steel - Satin',(#16871));
#16863=FILL_AREA_STYLE('Gray',(#16872));
#16864=FILL_AREA_STYLE('Opaque(147,158,163)',(#16873));
#16865=FILL_AREA_STYLE('Light Gray',(#16874));
#16866=FILL_AREA_STYLE('Dark Blue',(#16875));
#16867=FILL_AREA_STYLE('Black',(#16876));
#16868=FILL_AREA_STYLE('Sky Blue',(#16877));
#16869=FILL_AREA_STYLE('Blue',(#16878));
#16870=FILL_AREA_STYLE('Light Blue',(#16879));
#16871=FILL_AREA_STYLE_COLOUR('Steel - Satin',#16880);
#16872=FILL_AREA_STYLE_COLOUR('Gray',#16881);
#16873=FILL_AREA_STYLE_COLOUR('Opaque(147,158,163)',#16882);
#16874=FILL_AREA_STYLE_COLOUR('Light Gray',#16883);
#16875=FILL_AREA_STYLE_COLOUR('Dark Blue',#16884);
#16876=FILL_AREA_STYLE_COLOUR('Black',#16885);
#16877=FILL_AREA_STYLE_COLOUR('Sky Blue',#16886);
#16878=FILL_AREA_STYLE_COLOUR('Blue',#16887);
#16879=FILL_AREA_STYLE_COLOUR('Light Blue',#16888);
#16880=COLOUR_RGB('Steel - Satin',0.627450980392157,0.627450980392157,0.627450980392157);
#16881=COLOUR_RGB('Gray',0.501960784313725,0.501960784313725,0.501960784313725);
#16882=COLOUR_RGB('Opaque(147,158,163)',0.576470588235294,0.619607843137255,
0.63921568627451);
#16883=COLOUR_RGB('Light Gray',0.827450980392157,0.827450980392157,0.827450980392157);
#16884=COLOUR_RGB('Dark Blue',0.,0.125490196078431,0.376470588235294);
#16885=COLOUR_RGB('Black',0.0784313725490196,0.0784313725490196,0.0784313725490196);
#16886=COLOUR_RGB('Sky Blue',0.529411764705882,0.807843137254902,0.92156862745098);
#16887=COLOUR_RGB('Blue',0.,0.4,0.8);
#16888=COLOUR_RGB('Light Blue',0.67843137254902,0.847058823529412,0.901960784313726);
ENDSEC;
END-ISO-10303-21;
